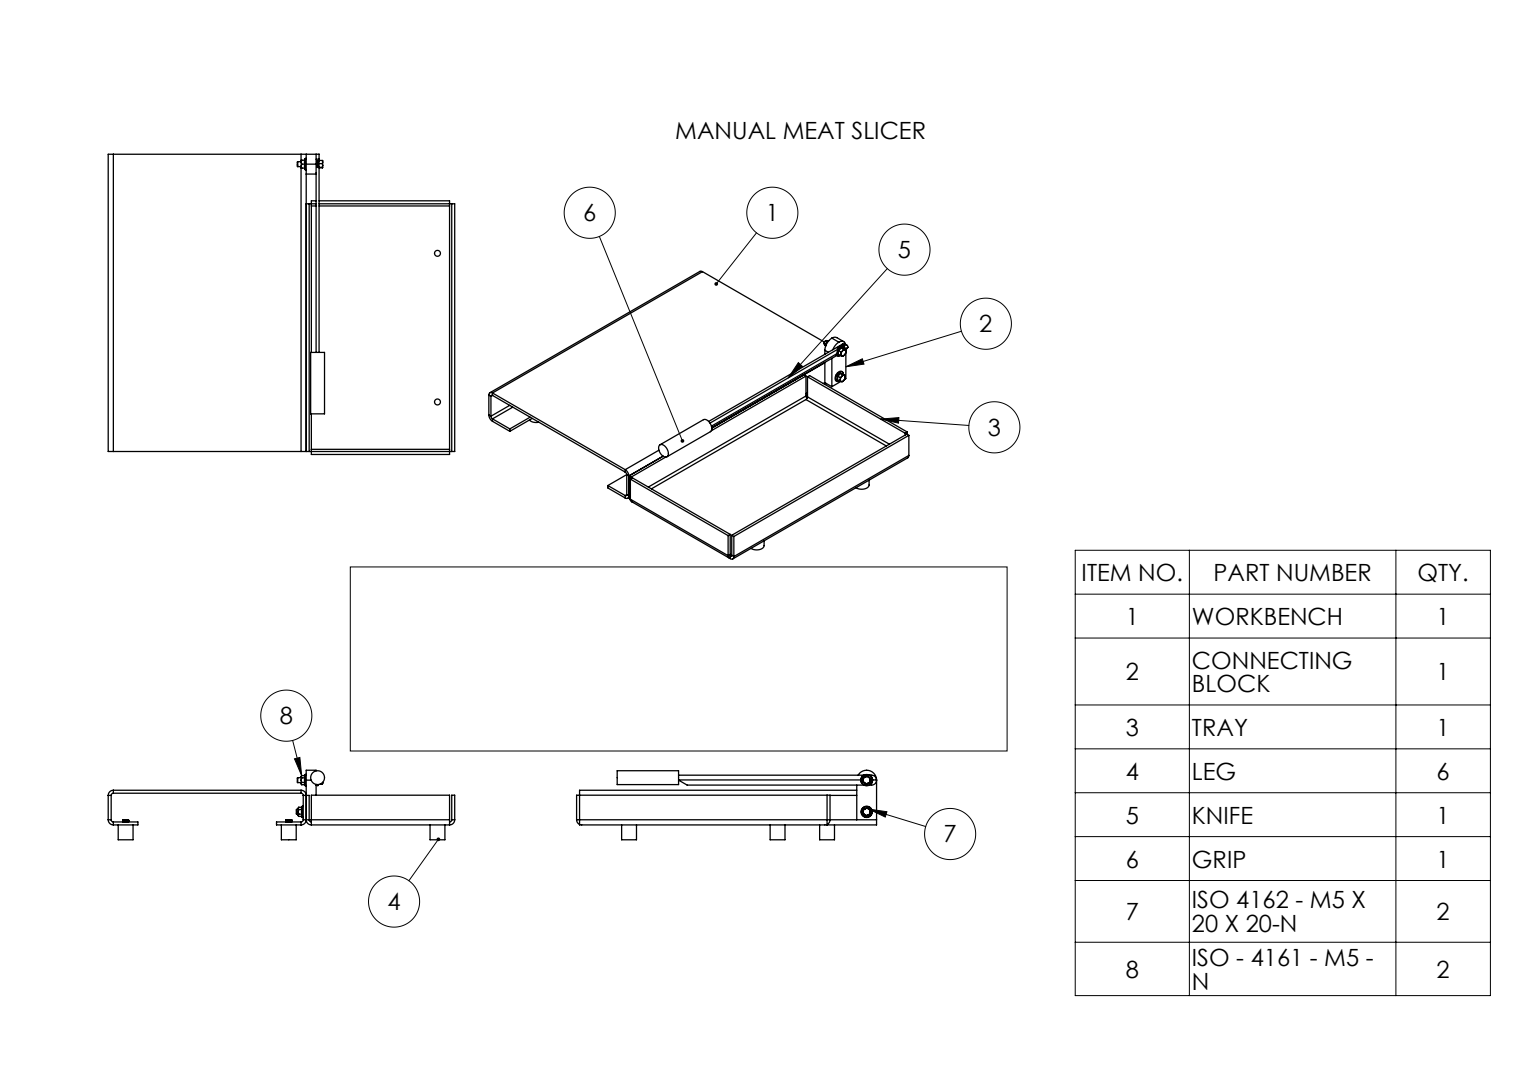
ISO-10303-21;
HEADER;
FILE_DESCRIPTION (('STEP AP214'),
    '1' );
FILE_NAME ('MAS-172',
    '2026-10-25T17:17:34',
    ( '' ),
    ( '' ),
    'SwSTEP 2.0',
    'SolidWorks 2026',
    '' );
FILE_SCHEMA (( 'AUTOMOTIVE_DESIGN' ));
ENDSEC;

DATA;
#1 = CARTESIAN_POINT ( 'NONE',  ( -79.64356964375001269, -33.59062499938548285, 98.40857419181659793 ) ) ;
#2 = CARTESIAN_POINT ( 'NONE',  ( 85.15643035625001289, -33.70312499938548711, 98.40857419181659793 ) ) ;
#3 = CARTESIAN_POINT ( 'NONE',  ( 82.39999999999999147, -32.36250000000000426, -96.99999999999997158 ) ) ;
#4 = DIRECTION ( 'NONE',  ( -0.000000000000000000, 0.8660254037844382635, 0.5000000000000006661 ) ) ;
#5 = CARTESIAN_POINT ( 'NONE',  ( 80.90000000000000568, -33.24374999877097281, -97.40192378864668399 ) ) ;
#6 = CARTESIAN_POINT ( 'NONE',  ( 231.0999999999999375, -32.62499999999999289, 102.5980762113533018 ) ) ;
#7 =( BOUNDED_SURFACE ( )  B_SPLINE_SURFACE ( 3, 2, ( 
 ( #3858, #16070, #12849 ),
 ( #17539, #18820, #1124 ),
 ( #12942, #8258, #11381 ),
 ( #11576, #9821, #15783 ),
 ( #19010, #5241, #9923 ),
 ( #17252, #845, #14308 ) ),
 .UNSPECIFIED., .F., .F., .F. ) 
 B_SPLINE_SURFACE_WITH_KNOTS ( ( 4, 2, 4 ),
 ( 3, 3 ),
 ( 0.02032853247518126918, 0.02278863295364821906, 0.02524873343211517240 ),
 ( 0.000000000000000000, 1.000000000000000000 ),
 .UNSPECIFIED. ) 
 GEOMETRIC_REPRESENTATION_ITEM ( )  RATIONAL_B_SPLINE_SURFACE ( (
 ( 1.000000000000000000, 0.8047781615896837382, 1.000000000000000000),
 ( 1.000000000000000000, 0.8123767586289252218, 1.000000000000000000),
 ( 1.000000000000000000, 0.8190662415564388121, 1.000000000000000000),
 ( 1.000000000000000000, 0.8192361015669026303, 1.000000000000000000),
 ( 1.000000000000000000, 0.8126135807103900266, 1.000000000000000000),
 ( 1.000000000000000000, 0.8047712338318593339, 1.000000000000000000) ) ) 
 REPRESENTATION_ITEM ( '' )  SURFACE ( )  );
#8 = ORIENTED_EDGE ( 'NONE', *, *, #12900, .F. ) ;
#9 = CARTESIAN_POINT ( 'NONE',  ( 4.175813232069147674, 2.061359961916367833, 3.570380186727398097 ) ) ;
#10 = CARTESIAN_POINT ( 'NONE',  ( 232.5999999999999375, -34.55624999877095860, 96.53589838486223584 ) ) ;
#11 = CARTESIAN_POINT ( 'NONE',  ( 234.0999999999999375, -32.34374999877096002, -52.59807621135342970 ) ) ;
#12 = CARTESIAN_POINT ( 'NONE',  ( -82.39999999999999147, -34.07812499938548711, 103.1828516163667899 ) ) ;
#13 = ORIENTED_EDGE ( 'NONE', *, *, #6864, .F. ) ;
#14 = VERTEX_POINT ( 'NONE', #6375 ) ;
#15 = CARTESIAN_POINT ( 'NONE',  ( -4.204015924366189871, 1.626724848190922446, -3.610627190413390419 ) ) ;
#16 = CARTESIAN_POINT ( 'NONE',  ( -85.39999999999999147, -34.97364041986484295, 98.90809577818235709 ) ) ;
#17 = CARTESIAN_POINT ( 'NONE',  ( -85.40000000000000568, -32.23124999877096997, 98.26794919243111792 ) ) ;
#18 = ORIENTED_EDGE ( 'NONE', *, *, #10099, .F. ) ;
#19 = CARTESIAN_POINT ( 'NONE',  ( -79.77811200999887831, -35.00000000000000000, 100.8506536761481414 ) ) ;
#20 = CARTESIAN_POINT ( 'NONE',  ( 82.40000000000000568, -30.00000000000000355, -103.0000000000000000 ) ) ;
#21 = CARTESIAN_POINT ( 'NONE',  ( -81.02178482187500208, -34.45312499938548711, 97.61286128772489690 ) ) ;
#22 = CARTESIAN_POINT ( 'NONE',  ( -79.39999999999999147, -33.41250000000000142, 101.7320508075688537 ) ) ;
#23 = CARTESIAN_POINT ( 'NONE',  ( -83.90000000000000568, -30.46874999877096712, 97.40192378864668399 ) ) ;
#24 = CARTESIAN_POINT ( 'NONE',  ( 231.7961524227065979, -33.50759618943233420, 103.0000000000000000 ) ) ;
#25 = CARTESIAN_POINT ( 'NONE',  ( 4.055492966679589806, 2.385006769472808319, 3.005124364834396822 ) ) ;
#26 = CARTESIAN_POINT ( 'NONE',  ( 0.000000000000000000, 0.000000000000000000, -0.2800830152838844622 ) ) ;
#27 = EDGE_CURVE ( 'NONE', #9630, #12897, #3914, .T. ) ;
#28 = CARTESIAN_POINT ( 'NONE',  ( 233.9782151781249411, -31.19062499938547717, 97.61286128772489690 ) ) ;
#29 = EDGE_LOOP ( 'NONE', ( #8971, #4412, #15076, #17801 ) ) ;
#30 = CARTESIAN_POINT ( 'NONE',  ( -85.15643035624999868, -34.22812499938547859, -101.5914258081833879 ) ) ;
#31 = CARTESIAN_POINT ( 'NONE',  ( 1.287237434362044075, 3.875615274277557809, -3.430618716626812059 ) ) ;
#32 = CARTESIAN_POINT ( 'NONE',  ( 233.4038475772933339, -34.57634618820330275, -53.00000000000011369 ) ) ;
#33 = CARTESIAN_POINT ( 'NONE',  ( 80.07894310789828296, -34.99999999999997868, -101.4973817956044400 ) ) ;
#34 = CARTESIAN_POINT ( 'NONE',  ( -85.15643035624999868, -31.00312499938548072, 101.5914258081833879 ) ) ;
#35 = CARTESIAN_POINT ( 'NONE',  ( 0.000000000000000000, 0.000000000000000000, -25.03750572909317285 ) ) ;
#36 = CARTESIAN_POINT ( 'NONE',  ( 233.9782151781249411, -32.54062499938547859, -52.38713871227520968 ) ) ;
#37 = ORIENTED_EDGE ( 'NONE', *, *, #1725, .T. ) ;
#38 = ORIENTED_EDGE ( 'NONE', *, *, #10348, .F. ) ;
#39 = CARTESIAN_POINT ( 'NONE',  ( -84.28136653320154892, -32.00000000000001421, 97.98546077809197641 ) ) ;
#40 = CARTESIAN_POINT ( 'NONE',  ( -85.40000000000000568, -31.38749999999999574, 98.26794919243111792 ) ) ;
#41 = CARTESIAN_POINT ( 'NONE',  ( -85.40000000000000568, -32.60624999877097707, 101.7320508075688679 ) ) ;
#42 = CARTESIAN_POINT ( 'NONE',  ( 82.39999999999999147, -32.36250000000000426, 103.4641016151377499 ) ) ;
#43 = CARTESIAN_POINT ( 'NONE',  ( -80.80636817121818183, -32.00000000000000000, -97.53037344451308854 ) ) ;
#44 = CARTESIAN_POINT ( 'NONE',  ( 235.3564303562499447, -33.92812499938548143, 98.40857419181659793 ) ) ;
#45 = CARTESIAN_POINT ( 'NONE',  ( 232.5999999999999943, -33.40312499938547575, -53.18285161636690361 ) ) ;
#46 = CARTESIAN_POINT ( 'NONE',  ( 82.39999999999999147, -33.62812499938549138, 96.81714838363319586 ) ) ;
#47 = EDGE_CURVE ( 'NONE', #12317, #11119, #12856, .T. ) ;
#48 = CARTESIAN_POINT ( 'NONE',  ( 85.15643035625001289, -30.59062499938548285, -99.99999999999998579 ) ) ;
#49 = ORIENTED_EDGE ( 'NONE', *, *, #18550, .F. ) ;
#50 =( BOUNDED_CURVE ( )  B_SPLINE_CURVE ( 2, ( #14072, #3327, #4905, #3619, #6463, #18477, #9481, #10851, #12417 ),
 .UNSPECIFIED., .F., .F. ) 
 B_SPLINE_CURVE_WITH_KNOTS ( ( 3, 2, 2, 2, 3 ),
 ( 0.6041666666666666297, 0.6111111111111111605, 0.6250000000000000000, 0.6388888888888888395, 0.6458333333333332593 ),
 .UNSPECIFIED. ) 
 CURVE ( )  GEOMETRIC_REPRESENTATION_ITEM ( )  RATIONAL_B_SPLINE_CURVE ( ( 0.9330127018922192983, 0.9330127018922187432, 1.000000000000000000, 0.8660254037844387076, 1.000000000000000000, 0.8660254037844387076, 1.000000000000000000, 0.9330127018922198534, 0.9330127018922192983 ) ) 
 REPRESENTATION_ITEM ( '' )  );
#51 = CARTESIAN_POINT ( 'NONE',  ( 235.3564303562499447, -34.41562499938547859, -50.00000000000011369 ) ) ;
#52 = CARTESIAN_POINT ( 'NONE',  ( 232.5999999999999375, -33.20624999877097139, 97.00000000000000000 ) ) ;
#53 = CARTESIAN_POINT ( 'NONE',  ( 83.77821517812500929, -34.26562499938548711, -97.61286128772489690 ) ) ;
#54 = EDGE_CURVE ( 'NONE', #12568, #18235, #14634, .T. ) ;
#55 = CYLINDRICAL_SURFACE ( 'NONE', #7872, 3.000000000000002665 ) ;
#56 = CARTESIAN_POINT ( 'NONE',  ( 233.9782151781249411, -31.90312499938548285, -47.61286128772501769 ) ) ;
#57 =( BOUNDED_CURVE ( )  B_SPLINE_CURVE ( 2, ( #14794, #2683, #1229, #10402, #2880, #14892, #1421, #4162, #17640 ),
 .UNSPECIFIED., .F., .F. ) 
 B_SPLINE_CURVE_WITH_KNOTS ( ( 3, 2, 2, 2, 3 ),
 ( 0.6458333333333333703, 0.6527777777777777901, 0.6666666666666666297, 0.6805555555555555802, 0.6875000000000000000 ),
 .UNSPECIFIED. ) 
 CURVE ( )  GEOMETRIC_REPRESENTATION_ITEM ( )  RATIONAL_B_SPLINE_CURVE ( ( 0.9330127018922192983, 0.9330127018922198534, 1.000000000000000000, 0.8660254037844387076, 1.000000000000000000, 0.8660254037844387076, 1.000000000000000000, 0.9330127018922194093, 0.9330127018922194093 ) ) 
 REPRESENTATION_ITEM ( '' )  );
#58 = CARTESIAN_POINT ( 'NONE',  ( -85.40000000000000568, -30.03750000000000497, 98.26794919243111792 ) ) ;
#59 = ORIENTED_EDGE ( 'NONE', *, *, #2774, .T. ) ;
#60 = CARTESIAN_POINT ( 'NONE',  ( -80.90000000000000568, -32.85000000000000142, 97.40192378864668399 ) ) ;
#61 = CARTESIAN_POINT ( 'NONE',  ( -79.39999999999999147, -31.03124999877097068, 98.26794919243110371 ) ) ;
#62 = DIRECTION ( 'NONE',  ( -0.000000000000000000, -0.000000000000000000, -1.000000000000000000 ) ) ;
#63 = CARTESIAN_POINT ( 'NONE',  ( -85.40000000000000568, -31.38356250001228531, 98.26794919243111792 ) ) ;
#64 = EDGE_CURVE ( 'NONE', #2579, #12229, #9687, .T. ) ;
#65 = LINE ( 'NONE', #3169, #11720 ) ;
#66 = PLANE ( 'NONE',  #10236 ) ;
#67 = CARTESIAN_POINT ( 'NONE',  ( -85.15643035624999868, -31.97812499938548925, 98.40857419181659793 ) ) ;
#68 = CARTESIAN_POINT ( 'NONE',  ( -79.39999999999999147, -32.47500000000000142, 99.99999999999998579 ) ) ;
#69 = CARTESIAN_POINT ( 'NONE',  ( 83.77821517812500929, -32.57812499938548711, 102.3871387122750889 ) ) ;
#70 = EDGE_CURVE ( 'NONE', #5083, #2374, #8515, .T. ) ;
#71 = B_SPLINE_CURVE_WITH_KNOTS ( 'NONE', 3,
 ( #6677, #3729, #9694, #17123, #815, #2842, #14458, #7240, #5600, #9889, #2460, #18880, #18782, #15852, #1291, #17315, #16038, #17507 ),
 .UNSPECIFIED., .F., .F.,
 ( 4, 2, 2, 2, 2, 2, 2, 2, 4 ),
 ( 0.000000000000000000, 0.0007106627595359568412, 0.001421325519071913682, 0.002131988278607870740, 0.002842651038143827365, 0.003553313797679783989, 0.004263976557215741481, 0.004974639316751698105, 0.005685302076287654729 ),
 .UNSPECIFIED. ) ;
#72 = CARTESIAN_POINT ( 'NONE',  ( 85.15643035625001289, -30.25312499938548783, -99.99999999999998579 ) ) ;
#73 = DIRECTION ( 'NONE',  ( -0.000000000000000000, -1.000000000000000000, -0.000000000000000000 ) ) ;
#74 = CARTESIAN_POINT ( 'NONE',  ( -83.77821517812500929, -32.87812499938548427, 102.3871387122750889 ) ) ;
#75 = CARTESIAN_POINT ( 'NONE',  ( -85.15643035624999868, -30.29062499938548925, -101.5914258081833879 ) ) ;
#76 = ORIENTED_EDGE ( 'NONE', *, *, #18961, .F. ) ;
#77 = CARTESIAN_POINT ( 'NONE',  ( 85.40000000000000568, -35.34374999877096712, 99.99999999999998579 ) ) ;
#78 = PLANE ( 'NONE',  #7094 ) ;
#79 = CARTESIAN_POINT ( 'NONE',  ( -82.40000000000000568, -30.00000000000000355, -96.99999999999998579 ) ) ;
#80 = VECTOR ( 'NONE', #9829, 1000.000000000000000 ) ;
#81 = CARTESIAN_POINT ( 'NONE',  ( -99.99999999999998579, -5.200000000000000178, 150.0000000000000000 ) ) ;
#82 = AXIS2_PLACEMENT_3D ( 'NONE', #16514, #3117, #16700 ) ;
#83 = CARTESIAN_POINT ( 'NONE',  ( -83.77821517812500929, -31.07812499938548711, 102.3871387122750889 ) ) ;
#84 =( BOUNDED_CURVE ( )  B_SPLINE_CURVE ( 2, ( #13183, #17688, #10354, #13091, #8980, #17790, #14840, #19061, #2929 ),
 .UNSPECIFIED., .F., .F. ) 
 B_SPLINE_CURVE_WITH_KNOTS ( ( 3, 2, 2, 2, 3 ),
 ( 0.7708333333333332593, 0.7777777777777777901, 0.7916666666666666297, 0.8055555555555555802, 0.8125000000000000000 ),
 .UNSPECIFIED. ) 
 CURVE ( )  GEOMETRIC_REPRESENTATION_ITEM ( )  RATIONAL_B_SPLINE_CURVE ( ( 0.9330127018922192983, 0.9330127018922187432, 1.000000000000000000, 0.8660254037844387076, 1.000000000000000000, 0.8660254037844387076, 1.000000000000000000, 0.9330127018922194093, 0.9330127018922194093 ) ) 
 REPRESENTATION_ITEM ( '' )  );
#85 = CARTESIAN_POINT ( 'NONE',  ( 82.61711639273572416, -31.99999999999999289, 102.8399189874672857 ) ) ;
#86 = ORIENTED_EDGE ( 'NONE', *, *, #4961, .F. ) ;
#87 = CARTESIAN_POINT ( 'NONE',  ( -83.90000000000000568, -30.82500000000000284, -97.40192378864668399 ) ) ;
#88 = CARTESIAN_POINT ( 'NONE',  ( 105.2000000000000455, -29.80000000000002203, 147.7999999999999829 ) ) ;
#89 = DIRECTION ( 'NONE',  ( 1.201851678989726239E-15, 0.8660254037844380415, -0.5000000000000009992 ) ) ;
#90 = CARTESIAN_POINT ( 'NONE',  ( -85.15643035625001289, -32.95312499938548711, -99.99999999999998579 ) ) ;
#91 = CARTESIAN_POINT ( 'NONE',  ( -82.14831453747900980, -32.00000000000000711, -102.8584433575392438 ) ) ;
#92 = CARTESIAN_POINT ( 'NONE',  ( 229.8435696437499303, -31.60312499938548214, 99.99999999999998579 ) ) ;
#93 = CARTESIAN_POINT ( 'NONE',  ( -79.39999999999999147, -32.91018749875867400, 101.7320508075688537 ) ) ;
#94 = APPLICATION_CONTEXT ( 'automotive_design' ) ;
#95 = CARTESIAN_POINT ( 'NONE',  ( -82.39999999999999147, -34.19062499938548427, 103.1828516163667899 ) ) ;
#96 = CARTESIAN_POINT ( 'NONE',  ( 233.4038475772933339, -33.67634618820329706, 96.99999999999998579 ) ) ;
#97 = CARTESIAN_POINT ( 'NONE',  ( 83.77821517812500929, -33.66562499938548569, 97.61286128772489690 ) ) ;
#98 = CARTESIAN_POINT ( 'NONE',  ( 80.90000000000000568, -32.40000000000000568, -97.40192378864668399 ) ) ;
#99 = AXIS2_PLACEMENT_3D ( 'NONE', #13083, #5582, #10259 ) ;
#100 = CARTESIAN_POINT ( 'NONE',  ( 232.5999999999999375, -33.43124999877096570, 102.9999999999999858 ) ) ;
#101 = EDGE_CURVE ( 'NONE', #1894, #1510, #1410, .T. ) ;
#102 = CARTESIAN_POINT ( 'NONE',  ( 83.90000000000000568, -35.26874999877097139, -102.5980762113533018 ) ) ;
#103 = CARTESIAN_POINT ( 'NONE',  ( 232.5999999999999375, -34.61249999999999716, 96.53589838486223584 ) ) ;
#104 = VERTEX_POINT ( 'NONE', #17014 ) ;
#105 = CARTESIAN_POINT ( 'NONE',  ( 231.2217848218749339, -34.22812499938548569, -47.61286128772501769 ) ) ;
#106 = DIRECTION ( 'NONE',  ( 0.000000000000000000, 0.000000000000000000, 1.000000000000000000 ) ) ;
#107 = CARTESIAN_POINT ( 'NONE',  ( 233.9782151781249411, -30.55312499938548143, 102.3871387122750889 ) ) ;
#108 = CARTESIAN_POINT ( 'NONE',  ( 229.5999999999999375, -33.99374999877096570, -50.00000000000011369 ) ) ;
#109 = CARTESIAN_POINT ( 'NONE',  ( -79.64356964374998427, -33.10312499938548569, 101.5914258081833879 ) ) ;
#110 = ORIENTED_EDGE ( 'NONE', *, *, #1169, .T. ) ;
#112 = ORIENTED_EDGE ( 'NONE', *, *, #10203, .F. ) ;
#111 = EDGE_CURVE ( 'NONE', #18607, #16633, #16646, .T. ) ;
#113 = CARTESIAN_POINT ( 'NONE',  ( -81.90908125319960220, -32.00000000000000711, 97.16185054498753004 ) ) ;
#114 = AXIS2_PLACEMENT_3D ( 'NONE', #4493, #4109, #5965 ) ;
#115 = CARTESIAN_POINT ( 'NONE',  ( -82.39999999999999147, -34.83749999999999858, 103.0000000000000000 ) ) ;
#116 = CARTESIAN_POINT ( 'NONE',  ( -79.39999999999999147, -34.76250000000000284, 101.7320508075688537 ) ) ;
#117 = ORIENTED_EDGE ( 'NONE', *, *, #1142, .T. ) ;
#118 = CARTESIAN_POINT ( 'NONE',  ( 69.99999999999998579, -31.99999999999998579, 150.0000000000000000 ) ) ;
#119 = CARTESIAN_POINT ( 'NONE',  ( 232.5999999999999375, -32.36249999999999716, 97.00000000000000000 ) ) ;
#120 = CARTESIAN_POINT ( 'NONE',  ( -85.15643035624999868, -33.44062499938548427, 98.40857419181659793 ) ) ;
#121 = CARTESIAN_POINT ( 'NONE',  ( -83.90000000000000568, -34.57500000000000284, 97.40192378864668399 ) ) ;
#122 = CARTESIAN_POINT ( 'NONE',  ( -79.39999999999999147, -31.93124999877096926, 98.26794919243110371 ) ) ;
#123 = FACE_OUTER_BOUND ( 'NONE', #5516, .T. ) ;
#124 =( BOUNDED_SURFACE ( )  B_SPLINE_SURFACE ( 1, 2, ( 
 ( #72, #18045, #10508, #17940, #4551, #3080, #4656, #1713, #12454, #13815, #2197, #651, #7770, #5135, #16858, #3463, #457, #16755, #7864, #15189, #8158, #2001, #1806, #6406, #9522, #9323, #14107, #17050, #9225, #11080, #551, #3563, #9626, #9421, #3371, #6508, #18420, #5041, #15389, #15287, #4754, #4848, #1902, #10982, #8060, #13913, #2100, #4947, #3269, #18518, #15588, #14015, #6599, #13723, #10793, #6699, #18329, #3661, #12361, #10890, #7958, #744, #364, #6313, #18135, #12266, #16951, #15487, #12547, #18231, #10698, #16664, #18617, #11277, #3951, #5339, #19004, #9815, #8536, #840, #5526, #6893, #1218, #6984, #14302, #2574, #12935, #5624, #16064, #14392, #1117, #18907, #15777, #18717, #3852, #17245, #2386, #12643, #12749, #8348, #11474, #4052, #15878, #938, #17441, #15685, #4148, #5235, #6803, #12843, #2482, #11183, #8440, #8253, #14486, #9719, #10011, #18812, #2669, #7077, #2289, #11570, #11375, #17341, #5436, #9916, #1031, #14203, #8629, #15969, #13033, #17533, #10108, #14587, #17147 ),
 ( #3754, #18022, #5908, #5808, #8918, #14880, #1509, #17822, #17733, #13124, #13221, #4340, #48, #16450, #2963, #10487, #13318, #11665, #7554, #4636, #3060, #9022, #16165, #19193, #15075, #7362, #148, #11759, #19295, #10301, #13511, #17628, #2776, #6099, #10201, #10391, #7459, #13419, #1318, #4243, #8729, #19094, #16260, #4433, #2870, #12047, #8827, #14981, #14683, #6000, #1409, #7174, #11950, #14784, #1605, #17920, #10586, #16551, #4529, #3150, #9113, #11854, #16352, #5715, #7266, #7751, #9602, #1786, #6293, #530, #12435, #4925, #16736, #15366, #4730, #12527, #7646, #15169, #15268, #10870, #13706, #6483, #3544, #1982, #15468, #346, #18116, #1883, #2078, #8035, #1694, #6581, #13601, #18403, #11059, #13992, #12244, #18211, #10964, #7940, #10772, #12341, #631, #3346, #5023, #4831, #18500, #9306, #10675, #440, #16841, #16644, #3447, #13891, #9500, #7842, #3640, #3246, #16934, #5119, #13797, #6385, #18305, #17030, #9402, #242, #6201, #12148, #9204, #17221, #8136, #18982, #17420, #4123, #2271 ) ),
 .UNSPECIFIED., .F., .F., .F. ) 
 B_SPLINE_SURFACE_WITH_KNOTS ( ( 2, 2 ),
 ( 3, 2, 2, 2, 2, 2, 2, 2, 2, 2, 2, 2, 2, 2, 2, 2, 2, 2, 2, 2, 2, 2, 2, 2, 2, 2, 2, 2, 2, 2, 2, 2, 2, 2, 2, 2, 2, 2, 2, 2, 2, 2, 2, 2, 2, 2, 2, 2, 2, 2, 2, 2, 2, 2, 2, 2, 2, 2, 2, 2, 2, 2, 2, 2, 2, 2, 2, 3 ),
 ( 0.000000000000000000, 1.000000000000000000 ),
 ( 0.000000000000000000, 0.01388888888888888812, 0.02777777777777777624, 0.04166666666666666435, 0.05555555555555555247, 0.06944444444444444753, 0.08333333333333332871, 0.09722222222222222376, 0.1111111111111111049, 0.1250000000000000000, 0.1388888888888888951, 0.1527777777777777901, 0.1666666666666666574, 0.1805555555555555525, 0.1944444444444444475, 0.2083333333333333426, 0.2222222222222222099, 0.2361111111111111049, 0.2500000000000000000, 0.2638888888888888951, 0.2777777777777777901, 0.2916666666666666852, 0.3055555555555555802, 0.3194444444444444198, 0.3333333333333333148, 0.3472222222222222099, 0.3611111111111111049, 0.3750000000000000000, 0.3888888888888888951, 0.4027777777777777901, 0.4166666666666666852, 0.4305555555555555802, 0.4444444444444444198, 0.4583333333333333148, 0.4722222222222222099, 0.4861111111111111049, 0.5000000000000000000, 0.5138888888888888395, 0.5277777777777777901, 0.5416666666666666297, 0.5555555555555555802, 0.5694444444444444198, 0.5833333333333333703, 0.5972222222222222099, 0.6111111111111111605, 0.6250000000000000000, 0.6388888888888888395, 0.6527777777777777901, 0.6666666666666666297, 0.6805555555555555802, 0.6944444444444444198, 0.7083333333333333703, 0.7222222222222222099, 0.7361111111111111605, 0.7500000000000000000, 0.7638888888888888395, 0.7777777777777777901, 0.7916666666666666297, 0.8055555555555555802, 0.8194444444444444198, 0.8333333333333333703, 0.8472222222222222099, 0.8611111111111111605, 0.8750000000000000000, 0.8888888888888888395, 0.9027777777777777901, 0.9166666666666666297, 0.9258785565094813652 ),
 .UNSPECIFIED. ) 
 GEOMETRIC_REPRESENTATION_ITEM ( )  RATIONAL_B_SPLINE_SURFACE ( (
 ( 1.000000000000000000, 0.8660254037844387076, 1.000000000000000000, 0.8660254037844387076, 1.000000000000000000, 0.8660254037844387076, 1.000000000000000000, 0.8660254037844387076, 1.000000000000000000, 0.8660254037844387076, 1.000000000000000000, 0.8660254037844387076, 1.000000000000000000, 0.8660254037844387076, 1.000000000000000000, 0.8660254037844387076, 1.000000000000000000, 0.8660254037844387076, 1.000000000000000000, 0.8660254037844387076, 1.000000000000000000, 0.8660254037844387076, 1.000000000000000000, 0.8660254037844387076, 1.000000000000000000, 0.8660254037844387076, 1.000000000000000000, 0.8660254037844387076, 1.000000000000000000, 0.8660254037844387076, 1.000000000000000000, 0.8660254037844387076, 1.000000000000000000, 0.8660254037844387076, 1.000000000000000000, 0.8660254037844387076, 1.000000000000000000, 0.8660254037844387076, 1.000000000000000000, 0.8660254037844387076, 1.000000000000000000, 0.8660254037844387076, 1.000000000000000000, 0.8660254037844387076, 1.000000000000000000, 0.8660254037844387076, 1.000000000000000000, 0.8660254037844387076, 1.000000000000000000, 0.8660254037844387076, 1.000000000000000000, 0.8660254037844387076, 1.000000000000000000, 0.8660254037844387076, 1.000000000000000000, 0.8660254037844387076, 1.000000000000000000, 0.8660254037844387076, 1.000000000000000000, 0.8660254037844387076, 1.000000000000000000, 0.8660254037844387076, 1.000000000000000000, 0.8660254037844387076, 1.000000000000000000, 0.8660254037844387076, 1.000000000000000000, 0.8660254037844387076, 1.000000000000000000, 0.8660254037844387076, 1.000000000000000000, 0.8660254037844387076, 1.000000000000000000, 0.8660254037844387076, 1.000000000000000000, 0.8660254037844387076, 1.000000000000000000, 0.8660254037844387076, 1.000000000000000000, 0.8660254037844387076, 1.000000000000000000, 0.8660254037844387076, 1.000000000000000000, 0.8660254037844387076, 1.000000000000000000, 0.8660254037844387076, 1.000000000000000000, 0.8660254037844387076, 1.000000000000000000, 0.8660254037844387076, 1.000000000000000000, 0.8660254037844387076, 1.000000000000000000, 0.8660254037844387076, 1.000000000000000000, 0.8660254037844387076, 1.000000000000000000, 0.8660254037844387076, 1.000000000000000000, 0.8660254037844387076, 1.000000000000000000, 0.8660254037844387076, 1.000000000000000000, 0.8660254037844387076, 1.000000000000000000, 0.8660254037844387076, 1.000000000000000000, 0.8660254037844387076, 1.000000000000000000, 0.8660254037844387076, 1.000000000000000000, 0.8660254037844387076, 1.000000000000000000, 0.8660254037844387076, 1.000000000000000000, 0.8660254037844387076, 1.000000000000000000, 0.8660254037844387076, 1.000000000000000000, 0.8660254037844387076, 1.000000000000000000, 0.8660254037844387076, 1.000000000000000000, 0.8660254037844387076, 1.000000000000000000, 0.8660254037844387076, 1.000000000000000000, 0.8660254037844387076, 1.000000000000000000, 0.8660254037844387076, 1.000000000000000000, 0.8660254037844387076, 1.000000000000000000, 0.9111405360107203144, 0.9401542295229963209),
 ( 1.000000000000000000, 0.8660254037844387076, 1.000000000000000000, 0.8660254037844387076, 1.000000000000000000, 0.8660254037844387076, 1.000000000000000000, 0.8660254037844387076, 1.000000000000000000, 0.8660254037844387076, 1.000000000000000000, 0.8660254037844387076, 1.000000000000000000, 0.8660254037844387076, 1.000000000000000000, 0.8660254037844387076, 1.000000000000000000, 0.8660254037844387076, 1.000000000000000000, 0.8660254037844387076, 1.000000000000000000, 0.8660254037844387076, 1.000000000000000000, 0.8660254037844387076, 1.000000000000000000, 0.8660254037844387076, 1.000000000000000000, 0.8660254037844387076, 1.000000000000000000, 0.8660254037844387076, 1.000000000000000000, 0.8660254037844387076, 1.000000000000000000, 0.8660254037844387076, 1.000000000000000000, 0.8660254037844387076, 1.000000000000000000, 0.8660254037844387076, 1.000000000000000000, 0.8660254037844387076, 1.000000000000000000, 0.8660254037844387076, 1.000000000000000000, 0.8660254037844387076, 1.000000000000000000, 0.8660254037844387076, 1.000000000000000000, 0.8660254037844387076, 1.000000000000000000, 0.8660254037844387076, 1.000000000000000000, 0.8660254037844387076, 1.000000000000000000, 0.8660254037844387076, 1.000000000000000000, 0.8660254037844387076, 1.000000000000000000, 0.8660254037844387076, 1.000000000000000000, 0.8660254037844387076, 1.000000000000000000, 0.8660254037844387076, 1.000000000000000000, 0.8660254037844387076, 1.000000000000000000, 0.8660254037844387076, 1.000000000000000000, 0.8660254037844387076, 1.000000000000000000, 0.8660254037844387076, 1.000000000000000000, 0.8660254037844387076, 1.000000000000000000, 0.8660254037844387076, 1.000000000000000000, 0.8660254037844387076, 1.000000000000000000, 0.8660254037844387076, 1.000000000000000000, 0.8660254037844387076, 1.000000000000000000, 0.8660254037844387076, 1.000000000000000000, 0.8660254037844387076, 1.000000000000000000, 0.8660254037844387076, 1.000000000000000000, 0.8660254037844387076, 1.000000000000000000, 0.8660254037844387076, 1.000000000000000000, 0.8660254037844387076, 1.000000000000000000, 0.8660254037844387076, 1.000000000000000000, 0.8660254037844387076, 1.000000000000000000, 0.8660254037844387076, 1.000000000000000000, 0.8660254037844387076, 1.000000000000000000, 0.8660254037844387076, 1.000000000000000000, 0.8660254037844387076, 1.000000000000000000, 0.8660254037844387076, 1.000000000000000000, 0.8660254037844387076, 1.000000000000000000, 0.8660254037844387076, 1.000000000000000000, 0.8660254037844387076, 1.000000000000000000, 0.8660254037844387076, 1.000000000000000000, 0.8660254037844387076, 1.000000000000000000, 0.8660254037844387076, 1.000000000000000000, 0.8660254037844387076, 1.000000000000000000, 0.8660254037844387076, 1.000000000000000000, 0.8660254037844387076, 1.000000000000000000, 0.8660254037844387076, 1.000000000000000000, 0.8660254037844387076, 1.000000000000000000, 0.8660254037844387076, 1.000000000000000000, 0.8660254037844387076, 1.000000000000000000, 0.9111405360107203144, 0.9401542295229963209) ) ) 
 REPRESENTATION_ITEM ( '' )  SURFACE ( )  );
#125 = CARTESIAN_POINT ( 'NONE',  ( 234.0999999999999375, -33.29999999999999716, 97.40192378864668399 ) ) ;
#126 = CARTESIAN_POINT ( 'NONE',  ( -80.90000000000000568, -33.45000000000000284, 102.5980762113533018 ) ) ;
#127 = CARTESIAN_POINT ( 'NONE',  ( -79.39999999999999147, -34.70624999877097139, -98.26794919243113213 ) ) ;
#128 = CARTESIAN_POINT ( 'NONE',  ( 229.8435696437499303, -31.04062499938547859, 99.99999999999998579 ) ) ;
#129 = ORIENTED_EDGE ( 'NONE', *, *, #8766, .F. ) ;
#130 = SHAPE_REPRESENTATION_RELATIONSHIP ( 'NONE' , 'NONE' ,  #4499, #5537 ) ;
#131 = CARTESIAN_POINT ( 'NONE',  ( -79.64356964374999848, -33.51562499938548711, -99.99999999999998579 ) ) ;
#132 = CARTESIAN_POINT ( 'NONE',  ( -82.65380294351676582, -34.99990492518305274, 97.01075526832239859 ) ) ;
#133 = CARTESIAN_POINT ( 'NONE',  ( 233.4038475772933054, -34.76115380933863008, -47.00000000000011369 ) ) ;
#134 = CARTESIAN_POINT ( 'NONE',  ( 81.96801452314025482, -35.00000000000000000, -102.7281823352556671 ) ) ;
#135 = CARTESIAN_POINT ( 'NONE',  ( -81.02178482187500208, -31.19062499938548427, 97.61286128772489690 ) ) ;
#136 = FACE_OUTER_BOUND ( 'NONE', #875, .T. ) ;
#137 = CARTESIAN_POINT ( 'NONE',  ( 233.9782151781249411, -32.24062499938548143, -47.61286128772501769 ) ) ;
#138 = VERTEX_POINT ( 'NONE', #3624 ) ;
#139 = EDGE_LOOP ( 'NONE', ( #12823, #17187, #7892, #9526 ) ) ;
#140 = CARTESIAN_POINT ( 'NONE',  ( -5.488773498207864225E-16, -2.859595677584339413, 2.047034997319579386 ) ) ;
#141 = CARTESIAN_POINT ( 'NONE',  ( -79.39999999999999147, -30.26249999999999929, 101.7320508075688537 ) ) ;
#142 = CARTESIAN_POINT ( 'NONE',  ( -79.39999999999999147, -32.90624999877096712, 101.7320508075688537 ) ) ;
#143 = CARTESIAN_POINT ( 'NONE',  ( 80.90000000000000568, -31.50000000000000000, 102.5980762113533018 ) ) ;
#144 = CARTESIAN_POINT ( 'NONE',  ( 244.7999999999999545, -32.00000000000000000, -100.0000000000000000 ) ) ;
#145 = CARTESIAN_POINT ( 'NONE',  ( 231.2217848218749339, -34.71562499938547575, 97.61286128772489690 ) ) ;
#146 = CARTESIAN_POINT ( 'NONE',  ( 83.90000000000000568, -32.11874999877097281, 97.40192378864668399 ) ) ;
#147 = CARTESIAN_POINT ( 'NONE',  ( 79.39999999999999147, -33.33749999999999858, -98.26794919243110371 ) ) ;
#148 = CARTESIAN_POINT ( 'NONE',  ( 83.77821517812500929, -31.11562499938548498, -97.61286128772489690 ) ) ;
#149 = ORIENTED_EDGE ( 'NONE', *, *, #9637, .F. ) ;
#150 = CARTESIAN_POINT ( 'NONE',  ( 235.5999999999999375, -32.47499999999999432, -50.00000000000011369 ) ) ;
#151 = CARTESIAN_POINT ( 'NONE',  ( 82.40000000000000568, -34.10624999877096997, 102.9999999999999858 ) ) ;
#152 = CARTESIAN_POINT ( 'NONE',  ( 79.64356964375001269, -34.37812499938548427, -98.40857419181659793 ) ) ;
#153 = CARTESIAN_POINT ( 'NONE',  ( -1.935715396507168721E-15, 2.686816014504566752, 2.346298152288372130 ) ) ;
#154 = CARTESIAN_POINT ( 'NONE',  ( -81.59615242270662350, -34.76115380933863719, 103.0000000000000000 ) ) ;
#155 = CARTESIAN_POINT ( 'NONE',  ( 229.8435696437499871, -31.11562499938547788, -48.40857419181671162 ) ) ;
#156 = CARTESIAN_POINT ( 'NONE',  ( -79.39999999999999147, -31.08750000000000213, 98.26794919243110371 ) ) ;
#157 = ORIENTED_EDGE ( 'NONE', *, *, #9586, .F. ) ;
#158 = DIRECTION ( 'NONE',  ( 0.000000000000000000, 1.000000000000000000, 0.000000000000000000 ) ) ;
#159 = CARTESIAN_POINT ( 'NONE',  ( 233.9782151781249411, -34.94062499938547717, 102.3871387122750889 ) ) ;
#160 = CARTESIAN_POINT ( 'NONE',  ( -79.39999999999999147, -32.43356250001229313, 98.26794919243110371 ) ) ;
#161 = EDGE_CURVE ( 'NONE', #11737, #9031, #8962, .T. ) ;
#162 = EDGE_CURVE ( 'NONE', #9344, #9023, #15270, .T. ) ;
#163 = DIRECTION ( 'NONE',  ( 1.000000000000000000, 0.000000000000000000, 0.000000000000000000 ) ) ;
#164 = CARTESIAN_POINT ( 'NONE',  ( -82.40000000000000568, -32.30624999877097281, 97.00000000000000000 ) ) ;
#165 = CARTESIAN_POINT ( 'NONE',  ( 230.0248882325332147, -35.00000000000000711, 98.48300226792288470 ) ) ;
#166 = CARTESIAN_POINT ( 'NONE',  ( 81.02178482187500208, -34.90312499938548285, 102.3871387122750889 ) ) ;
#167 = DIRECTION ( 'NONE',  ( 0.000000000000000000, 0.000000000000000000, 1.000000000000000000 ) ) ;
#168 = CARTESIAN_POINT ( 'NONE',  ( 0.000000000000000000, 0.000000000000000000, 0.000000000000000000 ) ) ;
#169 = CARTESIAN_POINT ( 'NONE',  ( -83.77821517812500929, -32.42812499938548854, 102.3871387122750889 ) ) ;
#170 = CARTESIAN_POINT ( 'NONE',  ( -81.02178482187500208, -30.55312499938548854, -97.61286128772489690 ) ) ;
#171 =( BOUNDED_CURVE ( )  B_SPLINE_CURVE ( 2, ( #17183, #11218, #2322, #15621, #3787, #16002, #5563, #9753, #17473 ),
 .UNSPECIFIED., .F., .F. ) 
 B_SPLINE_CURVE_WITH_KNOTS ( ( 3, 2, 2, 2, 3 ),
 ( 0.7291666666666668517, 0.7361111111111111605, 0.7500000000000000000, 0.7638888888888888395, 0.7708333333333332593 ),
 .UNSPECIFIED. ) 
 CURVE ( )  GEOMETRIC_REPRESENTATION_ITEM ( )  RATIONAL_B_SPLINE_CURVE ( ( 0.9330127018922194093, 0.9330127018922209636, 1.000000000000000000, 0.8660254037844387076, 1.000000000000000000, 0.8660254037844387076, 1.000000000000000000, 0.9330127018922198534, 0.9330127018922192983 ) ) 
 REPRESENTATION_ITEM ( '' )  );
#172 = ORIENTED_EDGE ( 'NONE', *, *, #15080, .F. ) ;
#173 = CARTESIAN_POINT ( 'NONE',  ( 83.77821517812500929, -31.07812499938548711, 97.61286128772489690 ) ) ;
#174 = CARTESIAN_POINT ( 'NONE',  ( -94.79999999999999716, -35.00000000000000000, 150.0000000000000000 ) ) ;
#175 = EDGE_CURVE ( 'NONE', #12231, #5767, #14452, .T. ) ;
#176 = VECTOR ( 'NONE', #9077, 1000.000000000000000 ) ;
#177 = SURFACE_SIDE_STYLE ('',( #16764 ) ) ;
#178 = EDGE_CURVE ( 'NONE', #2762, #9031, #12708, .T. ) ;
#179 = CARTESIAN_POINT ( 'NONE',  ( -81.02178482187500208, -31.30312499938548498, 97.61286128772489690 ) ) ;
#180 = CARTESIAN_POINT ( 'NONE',  ( 109.9999999999999432, -29.80000000000002558, -150.0000000000000000 ) ) ;
#181 = ORIENTED_EDGE ( 'NONE', *, *, #9607, .T. ) ;
#182 = CARTESIAN_POINT ( 'NONE',  ( -79.39999999999999147, -32.06250000000000000, -98.26794919243113213 ) ) ;
#183 = CARTESIAN_POINT ( 'NONE',  ( 4.000000000000000000, 2.512223110932545023, -3.469391141908803711 ) ) ;
#184 = DIRECTION ( 'NONE',  ( 1.000000000000000000, -2.001604010742470847E-15, 0.000000000000000000 ) ) ;
#185 = CARTESIAN_POINT ( 'NONE',  ( -81.02178482187500208, -32.35312499938548569, -97.61286128772489690 ) ) ;
#186 = CARTESIAN_POINT ( 'NONE',  ( 232.5999999999999375, -34.61249999999999716, -53.00000000000011369 ) ) ;
#187 = EDGE_CURVE ( 'NONE', #10576, #17634, #10361, .T. ) ;
#188 = CARTESIAN_POINT ( 'NONE',  ( 233.9782151781249411, -32.35312499938547859, 102.3871387122750889 ) ) ;
#189 = CARTESIAN_POINT ( 'NONE',  ( -80.90000000000000568, -32.49768749875867968, 102.5980762113533018 ) ) ;
#190 = CARTESIAN_POINT ( 'NONE',  ( -83.77821517812500929, -33.02812499938548285, 97.61286128772489690 ) ) ;
#191 = CARTESIAN_POINT ( 'NONE',  ( -85.15643035625001289, -34.60312499938548569, -98.40857419181659793 ) ) ;
#192 = CARTESIAN_POINT ( 'NONE',  ( 85.15643035625001289, -34.22812499938548569, 101.5914258081833879 ) ) ;
#193 = CARTESIAN_POINT ( 'NONE',  ( -5.384454397937118664, 6.702023979852544604E-16, -5.000000000000000000 ) ) ;
#194 = CIRCLE ( 'NONE', #8915, 2.199999999999993516 ) ;
#195 = DIRECTION ( 'NONE',  ( 1.000000000000000000, 0.000000000000000000, -0.000000000000000000 ) ) ;
#196 = CARTESIAN_POINT ( 'NONE',  ( 82.39999999999999147, -33.43124999877097281, -103.4641016151377499 ) ) ;
#197 = CARTESIAN_POINT ( 'NONE',  ( 235.5999999999999943, -34.76249999999999574, 101.7320508075688537 ) ) ;
#198 = VERTEX_POINT ( 'NONE', #5871 ) ;
#199 = CARTESIAN_POINT ( 'NONE',  ( 231.2217848218749339, -34.37812499938547717, -52.38713871227520968 ) ) ;
#200 = CARTESIAN_POINT ( 'NONE',  ( 116.6000000000000085, 10.19999999999994600, -140.0000000000000000 ) ) ;
#201 = CARTESIAN_POINT ( 'NONE',  ( 229.8435696437499871, -30.66562499938547859, 101.5914258081833879 ) ) ;
#202 = CARTESIAN_POINT ( 'NONE',  ( 229.5999999999999375, -33.95624999877095718, -48.26794919243123161 ) ) ;
#203 = CARTESIAN_POINT ( 'NONE',  ( -83.77821517812500929, -33.36562499938548854, 97.61286128772489690 ) ) ;
#204 = EDGE_LOOP ( 'NONE', ( #12601, #4330, #15037, #10087 ) ) ;
#205 = ORIENTED_EDGE ( 'NONE', *, *, #14467, .T. ) ;
#206 = CARTESIAN_POINT ( 'NONE',  ( 4.071447262713887127, 2.020725942163686728, -3.499999999999999556 ) ) ;
#207 = CARTESIAN_POINT ( 'NONE',  ( 105.1999999999999886, -29.80000000000002203, -100.0000000000000142 ) ) ;
#208 = ORIENTED_EDGE ( 'NONE', *, *, #11264, .T. ) ;
#209 = FACE_OUTER_BOUND ( 'NONE', #12612, .T. ) ;
#210 = CARTESIAN_POINT ( 'NONE',  ( 99.99999999999994316, -29.80000000000000782, -150.0000000000000000 ) ) ;
#211 = CARTESIAN_POINT ( 'NONE',  ( -85.15643035625001289, -33.40312499938548285, 99.99999999999998579 ) ) ;
#212 = CARTESIAN_POINT ( 'NONE',  ( -85.40000000000000568, -30.35045094645306563, 101.9998975609119469 ) ) ;
#213 = CARTESIAN_POINT ( 'NONE',  ( -82.39999999999999147, -30.73124999877096641, 103.4641016151377499 ) ) ;
#214 = CARTESIAN_POINT ( 'NONE',  ( 229.5999999999999375, -33.60000000000000142, 99.99999999999998579 ) ) ;
#215 = AXIS2_PLACEMENT_3D ( 'NONE', #7607, #13659, #15226 ) ;
#216 = CARTESIAN_POINT ( 'NONE',  ( -82.39999999999999147, -35.09062499938548285, 103.1828516163667899 ) ) ;
#217 = EDGE_CURVE ( 'NONE', #4443, #15882, #16415, .T. ) ;
#218 = CARTESIAN_POINT ( 'NONE',  ( 82.39999999999999147, -34.83749999999999858, -103.0000000000000000 ) ) ;
#219 = CARTESIAN_POINT ( 'NONE',  ( 3.948103430090399879, 3.379418997638482747, 1.146674596026232784 ) ) ;
#220 = CARTESIAN_POINT ( 'NONE',  ( -82.40000000000000568, -30.00000000000000355, -103.0000000000000000 ) ) ;
#221 = CARTESIAN_POINT ( 'NONE',  ( 235.3564303562499447, -32.16562499938547859, 99.99999999999998579 ) ) ;
#222 = ORIENTED_EDGE ( 'NONE', *, *, #5417, .T. ) ;
#223 = SHAPE_REPRESENTATION_RELATIONSHIP ( 'NONE' , 'NONE' ,  #14995, #14131 ) ;
#224 = CARTESIAN_POINT ( 'NONE',  ( -85.15643035625001289, -33.29062499938547859, -99.99999999999998579 ) ) ;
#225 = CARTESIAN_POINT ( 'NONE',  ( 3.453038570460273071, 2.625189405340834448, -3.535263753543585352 ) ) ;
#226 = CARTESIAN_POINT ( 'NONE',  ( 235.5999999999999375, -33.82499999999999574, 99.99999999999998579 ) ) ;
#227 = LINE ( 'NONE', #4417, #3668 ) ;
#228 = CARTESIAN_POINT ( 'NONE',  ( 230.7429016803109221, -35.00000000000000711, -47.88253972981398476 ) ) ;
#229 = LINE ( 'NONE', #334, #1662 ) ;
#230 = ORIENTED_EDGE ( 'NONE', *, *, #9491, .F. ) ;
#231 = ORIENTED_EDGE ( 'NONE', *, *, #3636, .T. ) ;
#232 = CARTESIAN_POINT ( 'NONE',  ( -83.74167325096719594, -31.99999999999997868, 102.4658751321106962 ) ) ;
#233 = CARTESIAN_POINT ( 'NONE',  ( -83.90000000000000568, -30.07499999999999929, 97.40192378864668399 ) ) ;
#234 = AXIS2_PLACEMENT_3D ( 'NONE', #19240, #195, #10724 ) ;
#235 = CARTESIAN_POINT ( 'NONE',  ( -83.90000000000000568, -30.91874999877096997, 97.40192378864668399 ) ) ;
#236 = CARTESIAN_POINT ( 'NONE',  ( 82.39999999999999147, -32.58750000000000568, 96.53589838486223584 ) ) ;
#237 = CARTESIAN_POINT ( 'NONE',  ( -80.42036527867321638, -32.00000000000000000, -97.80162405160960759 ) ) ;
#238 = CARTESIAN_POINT ( 'NONE',  ( 229.8435696437499303, -33.29062499938547148, 99.99999999999998579 ) ) ;
#239 = CARTESIAN_POINT ( 'NONE',  ( 231.7960411235079050, -35.00000000000002132, -47.36341917746382535 ) ) ;
#240 = VECTOR ( 'NONE', #19274, 1000.000000000000000 ) ;
#241 = CARTESIAN_POINT ( 'NONE',  ( 81.59615242270662350, -33.46740381056766722, -102.9999999999999716 ) ) ;
#242 = CARTESIAN_POINT ( 'NONE',  ( 79.64356964375001269, -34.82812499938548711, -98.40857419181659793 ) ) ;
#243 = ORIENTED_EDGE ( 'NONE', *, *, #11982, .F. ) ;
#244 = CARTESIAN_POINT ( 'NONE',  ( 229.5999999999999375, -32.21249999999999858, -48.26794919243123161 ) ) ;
#245 = CARTESIAN_POINT ( 'NONE',  ( -80.90000000000000568, -31.59374999877097423, 102.5980762113533018 ) ) ;
#246 = CARTESIAN_POINT ( 'NONE',  ( 85.15643035624999868, -33.77812499938548285, -98.40857419181659793 ) ) ;
#247 = VECTOR ( 'NONE', #7483, 1000.000000000000000 ) ;
#248 = STYLED_ITEM ( 'NONE', ( #13866 ), #18578 ) ;
#249 = CARTESIAN_POINT ( 'NONE',  ( 94.79999999999995453, -29.80000000000000071, 150.0000000000000000 ) ) ;
#250 = CARTESIAN_POINT ( 'NONE',  ( -83.77821517812500929, -31.52812499938548996, 102.3871387122750889 ) ) ;
#251 = CARTESIAN_POINT ( 'NONE',  ( 233.9782151781249411, -33.70312499938548001, -47.61286128772501769 ) ) ;
#252 = CARTESIAN_POINT ( 'NONE',  ( -80.90000000000000568, -30.75000000000000355, 102.5980762113533018 ) ) ;
#253 = ORIENTED_EDGE ( 'NONE', *, *, #17135, .F. ) ;
#254 = CARTESIAN_POINT ( 'NONE',  ( -82.31848699153323423, -34.99951142137499716, 103.0191144166183221 ) ) ;
#255 = ADVANCED_FACE ( 'NONE', ( #14648 ), #17592, .T. ) ;
#256 = AXIS2_PLACEMENT_3D ( 'NONE', #7391, #10235, #1349 ) ;
#257 = DIRECTION ( 'NONE',  ( 0.000000000000000000, 0.000000000000000000, -1.000000000000000000 ) ) ;
#258 = CARTESIAN_POINT ( 'NONE',  ( 79.64356964375001269, -30.85312499938548569, 98.40857419181659793 ) ) ;
#259 = CARTESIAN_POINT ( 'NONE',  ( -85.40000000000000568, -34.96970290221972277, 98.90809659374338025 ) ) ;
#260 = CIRCLE ( 'NONE', #11165, 5.000000000000000000 ) ;
#261 = CARTESIAN_POINT ( 'NONE',  ( -1.999999999999999556, 3.464101615137754830, -3.142992957459232795 ) ) ;
#262 = CARTESIAN_POINT ( 'NONE',  ( -79.64356964374998427, -30.51562499938548711, 101.5914258081833879 ) ) ;
#263 = CARTESIAN_POINT ( 'NONE',  ( 85.12124608221321864, -31.99999999999999289, 100.4735569575797030 ) ) ;
#264 = CARTESIAN_POINT ( 'NONE',  ( 83.77821517812500929, -33.92812499938548854, 102.3871387122750889 ) ) ;
#265 = CARTESIAN_POINT ( 'NONE',  ( -2.100000000000000089, 2.571758278209441957E-16, -5.000000000000000000 ) ) ;
#266 = AXIS2_PLACEMENT_3D ( 'NONE', #8263, #12758, #18727 ) ;
#267 = CARTESIAN_POINT ( 'NONE',  ( 235.5999999999999943, -32.96249999999999858, -48.26794919243124582 ) ) ;
#268 = CARTESIAN_POINT ( 'NONE',  ( -84.74067385206558356, -32.00000000000000000, -101.4666071953143529 ) ) ;
#269 = CARTESIAN_POINT ( 'NONE',  ( -79.64356964374999848, -34.52812499938548285, -99.99999999999998579 ) ) ;
#270 = PRODUCT_DEFINITION_CONTEXT ( 'detailed design', #8572, 'design' ) ;
#271 = ORIENTED_EDGE ( 'NONE', *, *, #3421, .F. ) ;
#272 = CARTESIAN_POINT ( 'NONE',  ( 79.64356964375001269, -31.41562499938548569, 98.40857419181659793 ) ) ;
#273 = CARTESIAN_POINT ( 'NONE',  ( 96.99999999999998579, 4.758098676964956264E-15, -150.0000000000000000 ) ) ;
#274 = AXIS2_PLACEMENT_3D ( 'NONE', #18067, #19141, #10151 ) ;
#275 = CARTESIAN_POINT ( 'NONE',  ( 4.114405500665261783, -2.025575754679711959, -3.508400121684924322 ) ) ;
#276 = VECTOR ( 'NONE', #14347, 1000.000000000000000 ) ;
#277 = CARTESIAN_POINT ( 'NONE',  ( -82.39999999999999147, -31.49062499938548854, 103.1828516163667899 ) ) ;
#278 = DIRECTION ( 'NONE',  ( 0.000000000000000000, -1.000000000000000000, 0.000000000000000000 ) ) ;
#279 = ORIENTED_EDGE ( 'NONE', *, *, #11777, .T. ) ;
#280 = CARTESIAN_POINT ( 'NONE',  ( -85.40000000000000568, -30.86250000000000071, -98.26794919243111792 ) ) ;
#281 = CARTESIAN_POINT ( 'NONE',  ( 85.40000000000000568, -34.46249999999999858, -101.7320508075688679 ) ) ;
#282 = DIRECTION ( 'NONE',  ( -1.000000000000000000, 0.000000000000000000, 0.000000000000000000 ) ) ;
#283 = CARTESIAN_POINT ( 'NONE',  ( -85.15643035624999868, -33.81562499938549138, -98.40857419181659793 ) ) ;
#284 = CARTESIAN_POINT ( 'NONE',  ( -0.5449313310646672903, -4.304185902836978883, -3.316620875263469159 ) ) ;
#285 = CARTESIAN_POINT ( 'NONE',  ( 232.5999999999999375, -33.74062499938548143, 103.1828516163667899 ) ) ;
#286 = CARTESIAN_POINT ( 'NONE',  ( -79.39999999999999147, -31.52268749875867471, 99.99999999999998579 ) ) ;
#287 = EDGE_LOOP ( 'NONE', ( #12680, #18333, #2040 ) ) ;
#288 = CARTESIAN_POINT ( 'NONE',  ( -82.39999999999999147, -33.74062499938548854, 103.1828516163667899 ) ) ;
#289 = CONICAL_SURFACE ( 'NONE', #10266, 4.000000000000000000, 0.8911886515913786111 ) ;
#290 = EDGE_CURVE ( 'NONE', #8383, #14066, #13875, .T. ) ;
#291 = CARTESIAN_POINT ( 'NONE',  ( -79.64356964374998427, -34.00312499938548427, -98.40857419181659793 ) ) ;
#292 = CARTESIAN_POINT ( 'NONE',  ( 82.39999999999999147, -34.30312499938548143, 103.1828516163667899 ) ) ;
#293 = CARTESIAN_POINT ( 'NONE',  ( 79.39999999999999147, -34.31250000000000000, 98.26794919243113213 ) ) ;
#294 =( BOUNDED_CURVE ( )  B_SPLINE_CURVE ( 2, ( #4333, #5428, #17722, #10192, #1107, #14385, #5519, #1310, #7258 ),
 .UNSPECIFIED., .F., .F. ) 
 B_SPLINE_CURVE_WITH_KNOTS ( ( 3, 2, 2, 2, 3 ),
 ( 0.3125000000000001665, 0.3194444444444444198, 0.3333333333333333148, 0.3472222222222222099, 0.3541666666666666297 ),
 .UNSPECIFIED. ) 
 CURVE ( )  GEOMETRIC_REPRESENTATION_ITEM ( )  RATIONAL_B_SPLINE_CURVE ( ( 0.9330127018922194093, 0.9330127018922209636, 1.000000000000000000, 0.8660254037844387076, 1.000000000000000000, 0.8660254037844387076, 1.000000000000000000, 0.9330127018922196314, 0.9330127018922194093 ) ) 
 REPRESENTATION_ITEM ( '' )  );
#295 = CARTESIAN_POINT ( 'NONE',  ( 110.9999999999999574, -21.80000000000003268, -142.6499999999999773 ) ) ;
#296 = CARTESIAN_POINT ( 'NONE',  ( 82.39999999999999147, -34.55624999877096570, -96.53589838486223584 ) ) ;
#297 = CARTESIAN_POINT ( 'NONE',  ( 234.0999999999999375, -34.35000000000000142, 102.5980762113533018 ) ) ;
#298 = ORIENTED_EDGE ( 'NONE', *, *, #2474, .F. ) ;
#299 = CARTESIAN_POINT ( 'NONE',  ( 235.3564303562499447, -34.04062499938548569, -51.59142580818350154 ) ) ;
#300 = CARTESIAN_POINT ( 'NONE',  ( 0.000000000000000000, 0.000000000000000000, 0.000000000000000000 ) ) ;
#301 = CARTESIAN_POINT ( 'NONE',  ( 232.5999999999999375, -31.04062499938547859, 103.1828516163667899 ) ) ;
#302 = CARTESIAN_POINT ( 'NONE',  ( 234.0999999999999375, -35.04374999877096286, -52.59807621135342970 ) ) ;
#303 = ADVANCED_FACE ( 'NONE', ( #13187 ), #10269, .F. ) ;
#304 = CARTESIAN_POINT ( 'NONE',  ( -85.15643035625001289, -35.05312499938548143, 101.5914258081833879 ) ) ;
#305 = ORIENTED_EDGE ( 'NONE', *, *, #12340, .T. ) ;
#306 = ORIENTED_EDGE ( 'NONE', *, *, #13225, .F. ) ;
#307 = CARTESIAN_POINT ( 'NONE',  ( 3.951447005078452701, -3.704664227300105583, 0.5833333333333329263 ) ) ;
#308 = CARTESIAN_POINT ( 'NONE',  ( -4.000000000000000000, 2.511478553582031203, -3.469254451724764543 ) ) ;
#309 = DIRECTION ( 'NONE',  ( -0.000000000000000000, -1.000000000000000000, -0.000000000000000000 ) ) ;
#310 = ORIENTED_EDGE ( 'NONE', *, *, #16679, .T. ) ;
#311 = CARTESIAN_POINT ( 'NONE',  ( -99.99999999999998579, -29.80000000000000426, 150.0000000000000000 ) ) ;
#312 = CARTESIAN_POINT ( 'NONE',  ( 229.5999999999999375, -34.03124999877096002, 98.26794919243111792 ) ) ;
#313 = DIRECTION ( 'NONE',  ( 1.000000000000000000, -1.387778780781445676E-15, -2.407412430484046130E-31 ) ) ;
#314 = CARTESIAN_POINT ( 'NONE',  ( -79.39999999999999147, -33.78750000000000142, 98.26794919243110371 ) ) ;
#315 = EDGE_CURVE ( 'NONE', #15577, #16231, #9273, .T. ) ;
#316 = CARTESIAN_POINT ( 'NONE',  ( -83.90000000000000568, -30.91874999877096997, 97.40192378864668399 ) ) ;
#317 = CARTESIAN_POINT ( 'NONE',  ( 235.2013144571816952, -32.00000000000002132, -51.47161334219405404 ) ) ;
#318 = ADVANCED_FACE ( 'NONE', ( #11630 ), #5967, .F. ) ;
#319 = CARTESIAN_POINT ( 'NONE',  ( -79.39999999999999147, -30.71250000000000213, 101.7320508075688537 ) ) ;
#320 = CARTESIAN_POINT ( 'NONE',  ( 82.40000000000000568, -34.61250000000001137, -97.00000000000000000 ) ) ;
#321 = CARTESIAN_POINT ( 'NONE',  ( -79.39999999999999147, -33.37500000000000000, 99.99999999999998579 ) ) ;
#322 = CARTESIAN_POINT ( 'NONE',  ( -82.40000000000000568, -30.00000000000000355, 103.0000000000000000 ) ) ;
#323 = EDGE_CURVE ( 'NONE', #14868, #14858, #1084, .T. ) ;
#324 = B_SPLINE_CURVE_WITH_KNOTS ( 'NONE', 3,
 ( #1017, #7159, #1300, #2555 ),
 .UNSPECIFIED., .F., .F.,
 ( 4, 4 ),
 ( 0.000000000000000000, 0.002080789711329297104 ),
 .UNSPECIFIED. ) ;
#325 = CARTESIAN_POINT ( 'NONE',  ( 229.8435696437499871, -32.42812499938548143, 98.40857419181659793 ) ) ;
#326 = ORIENTED_EDGE ( 'NONE', *, *, #4980, .F. ) ;
#327 = FILL_AREA_STYLE ('',( #7917 ) ) ;
#328 = CARTESIAN_POINT ( 'NONE',  ( -85.15643035624999868, -32.35312499938549280, -98.40857419181659793 ) ) ;
#329 = DIRECTION ( 'NONE',  ( -0.000000000000000000, -1.000000000000000000, -0.000000000000000000 ) ) ;
#330 = ORIENTED_EDGE ( 'NONE', *, *, #12340, .F. ) ;
#331 = DIRECTION ( 'NONE',  ( 1.000000000000000000, 0.000000000000000000, 0.000000000000000000 ) ) ;
#332 = CARTESIAN_POINT ( 'NONE',  ( 0.000000000000000000, 0.000000000000000000, 2.500000000000000444 ) ) ;
#333 = CARTESIAN_POINT ( 'NONE',  ( 231.5655627039840567, -35.00000000000000000, -47.42249611015796518 ) ) ;
#334 = CARTESIAN_POINT ( 'NONE',  ( 102.9999999999999858, -29.80000000000000071, -100.0000000000000000 ) ) ;
#335 = ORIENTED_EDGE ( 'NONE', *, *, #6417, .T. ) ;
#336 = EDGE_LOOP ( 'NONE', ( #9804, #7178, #6008, #18106, #9174, #4508, #17848 ) ) ;
#337 = CARTESIAN_POINT ( 'NONE',  ( 79.39999999999999147, -34.63124999877096855, 101.7320508075688963 ) ) ;
#338 = EDGE_CURVE ( 'NONE', #8719, #3780, #14563, .T. ) ;
#339 = CARTESIAN_POINT ( 'NONE',  ( 82.39999999999999147, -34.97812499938547859, -103.1828516163667899 ) ) ;
#340 = CARTESIAN_POINT ( 'NONE',  ( -79.39999999999999147, -31.03124999877097068, 98.26794919243110371 ) ) ;
#341 = CARTESIAN_POINT ( 'NONE',  ( 85.40000000000000568, -32.25000000000000000, 99.99999999999998579 ) ) ;
#342 = CARTESIAN_POINT ( 'NONE',  ( -83.52979456739218733, -32.00000000000002132, -97.41965524898077433 ) ) ;
#343 = CARTESIAN_POINT ( 'NONE',  ( 229.8435696437499871, -33.77812499938548285, 98.40857419181659793 ) ) ;
#344 = CARTESIAN_POINT ( 'NONE',  ( 83.77821517812500929, -32.42812499938548854, -102.3871387122750889 ) ) ;
#345 = CARTESIAN_POINT ( 'NONE',  ( 82.40000000000000568, -30.00000000000000355, 99.99999999999998579 ) ) ;
#346 = CARTESIAN_POINT ( 'NONE',  ( 85.15643035624999868, -33.32812499938548001, -98.40857419181659793 ) ) ;
#347 = ORIENTED_EDGE ( 'NONE', *, *, #19285, .F. ) ;
#348 = CARTESIAN_POINT ( 'NONE',  ( 235.5999999999999943, -33.78749999999999432, -51.73205080756900287 ) ) ;
#349 = ADVANCED_FACE ( 'NONE', ( #13762 ), #13787, .T. ) ;
#350 = CARTESIAN_POINT ( 'NONE',  ( -83.20384757729335945, -34.14240381056767148, 96.99999999999998579 ) ) ;
#351 = CARTESIAN_POINT ( 'NONE',  ( -85.40000000000000568, -34.08749999999999858, 98.26794919243111792 ) ) ;
#352 = DIRECTION ( 'NONE',  ( 0.000000000000000000, -1.000000000000000000, 0.000000000000000000 ) ) ;
#353 = CARTESIAN_POINT ( 'NONE',  ( -83.77821517812500929, -30.32812499938548711, 97.61286128772489690 ) ) ;
#354 = CARTESIAN_POINT ( 'NONE',  ( 235.3564303562499447, -33.14062499938548001, -51.59142580818350865 ) ) ;
#355 = CARTESIAN_POINT ( 'NONE',  ( -85.15643035624999868, -34.60312499938548569, 101.5914258081833879 ) ) ;
#356 = ORIENTED_EDGE ( 'NONE', *, *, #12713, .T. ) ;
#357 = CARTESIAN_POINT ( 'NONE',  ( -79.76502430829106061, -35.00019033771674515, 98.52379045060148144 ) ) ;
#358 = CARTESIAN_POINT ( 'NONE',  ( 232.5999999999999943, -34.30312499938547433, 96.81714838363319586 ) ) ;
#359 = CARTESIAN_POINT ( 'NONE',  ( 83.77821517812500929, -31.11562499938548498, 102.3871387122750889 ) ) ;
#360 = CARTESIAN_POINT ( 'NONE',  ( 235.5999999999999943, -34.76249999999999574, 101.7320508075688537 ) ) ;
#361 = CARTESIAN_POINT ( 'NONE',  ( -83.77821517812500929, -31.07812499938548711, 102.3871387122750889 ) ) ;
#362 = CARTESIAN_POINT ( 'NONE',  ( 235.5999999999999375, -32.01330983656912821, 99.46005447970520663 ) ) ;
#363 = CARTESIAN_POINT ( 'NONE',  ( 79.64356964374999848, -30.81562499938548427, 99.99999999999998579 ) ) ;
#364 = CARTESIAN_POINT ( 'NONE',  ( 83.77821517812500929, -32.57812499938548711, -97.61286128772489690 ) ) ;
#365 = CARTESIAN_POINT ( 'NONE',  ( 229.8435696437499303, -30.59062499938547575, -50.00000000000011369 ) ) ;
#366 = CARTESIAN_POINT ( 'NONE',  ( -84.67508262029694777, -32.00000000000000711, -98.43364869553373353 ) ) ;
#367 = CARTESIAN_POINT ( 'NONE',  ( -82.39999999999999147, -33.74062499938548854, -96.81714838363319586 ) ) ;
#368 = ORIENTED_EDGE ( 'NONE', *, *, #16035, .T. ) ;
#369 = CARTESIAN_POINT ( 'NONE',  ( 80.90000000000000568, -34.59374999877096712, 102.5980762113533018 ) ) ;
#370 = CARTESIAN_POINT ( 'NONE',  ( 232.5999999999999091, -34.38749999999999574, 102.9999999999999858 ) ) ;
#371 = CARTESIAN_POINT ( 'NONE',  ( -85.40000000000000568, -33.18750000000000000, 98.26794919243111792 ) ) ;
#372 = CARTESIAN_POINT ( 'NONE',  ( -83.77821517812500929, -34.37812499938548427, 97.61286128772489690 ) ) ;
#373 = CARTESIAN_POINT ( 'NONE',  ( 118.5000000000000284, 12.69999999999998508, 50.00000000000001421 ) ) ;
#374 = ORIENTED_EDGE ( 'NONE', *, *, #7762, .F. ) ;
#375 = CARTESIAN_POINT ( 'NONE',  ( -83.90000000000000568, -30.52500000000000213, -102.5980762113533018 ) ) ;
#376 = CARTESIAN_POINT ( 'NONE',  ( 83.04276107155152431, -34.99999999999999289, 102.9375709370400642 ) ) ;
#377 = CARTESIAN_POINT ( 'NONE',  ( 80.08630547029493130, -32.02340763552834346, -102.1282894555899361 ) ) ;
#378 = FACE_OUTER_BOUND ( 'NONE', #12586, .T. ) ;
#379 = CARTESIAN_POINT ( 'NONE',  ( 235.3564303562499447, -34.97812499938547859, 99.99999999999998579 ) ) ;
#380 = CARTESIAN_POINT ( 'NONE',  ( -80.90000000000000568, -35.19768749875867542, 102.5980762113533018 ) ) ;
#381 = EDGE_LOOP ( 'NONE', ( #16724, #7367, #9403, #6838, #9257, #5214, #15859, #12633, #9758, #10396, #17402, #15523, #2220, #3836, #18473, #563, #7521 ) ) ;
#382 = DIRECTION ( 'NONE',  ( -1.000000000000000000, 1.387778780781445676E-15, 2.407412430484046130E-31 ) ) ;
#383 = LINE ( 'NONE', #15609, #4157 ) ;
#384 = CARTESIAN_POINT ( 'NONE',  ( 79.64356964374998427, -32.57812499938548711, 101.5914258081833879 ) ) ;
#385 = CARTESIAN_POINT ( 'NONE',  ( 232.5999999999999375, -29.99999999999999645, -47.00000000000010658 ) ) ;
#386 = FACE_OUTER_BOUND ( 'NONE', #3807, .T. ) ;
#387 = CARTESIAN_POINT ( 'NONE',  ( 83.90000000000000568, -34.51874999877097139, -97.40192378864668399 ) ) ;
#388 = CYLINDRICAL_SURFACE ( 'NONE', #13636, 3.000000000000002665 ) ;
#389 = AXIS2_PLACEMENT_3D ( 'NONE', #88, #5845, #13359 ) ;
#390 = VECTOR ( 'NONE', #16629, 1000.000000000000000 ) ;
#391 = ORIENTED_EDGE ( 'NONE', *, *, #17376, .F. ) ;
#392 = CARTESIAN_POINT ( 'NONE',  ( 235.3564303562499447, -32.27812499938548285, -50.00000000000011369 ) ) ;
#393 = CARTESIAN_POINT ( 'NONE',  ( 233.9782151781249411, -31.30312499938547788, 97.61286128772489690 ) ) ;
#394 = CARTESIAN_POINT ( 'NONE',  ( 229.8435696437499303, -30.25312499938548072, -50.00000000000011369 ) ) ;
#395 = CARTESIAN_POINT ( 'NONE',  ( -81.59615242270662350, -33.01740381056767148, -96.99999999999998579 ) ) ;
#396 = ORIENTED_EDGE ( 'NONE', *, *, #404, .T. ) ;
#397 = ORIENTED_EDGE ( 'NONE', *, *, #4624, .T. ) ;
#398 = CARTESIAN_POINT ( 'NONE',  ( 4.211140560182196957, 2.431303136016536470, -3.745885042887433514 ) ) ;
#399 = CARTESIAN_POINT ( 'NONE',  ( -81.59615242270665192, -33.86115380933864571, -97.00000000000000000 ) ) ;
#400 = DIRECTION ( 'NONE',  ( 0.000000000000000000, 0.000000000000000000, 1.000000000000000000 ) ) ;
#401 = ORIENTED_EDGE ( 'NONE', *, *, #14601, .T. ) ;
#402 = CARTESIAN_POINT ( 'NONE',  ( 85.15643035625001289, -32.09062499938548996, 101.5914258081833879 ) ) ;
#403 = CARTESIAN_POINT ( 'NONE',  ( -80.90000000000000568, -32.79374999877096997, -102.5980762113533018 ) ) ;
#404 = EDGE_CURVE ( 'NONE', #11560, #13270, #807, .T. ) ;
#405 = AXIS2_PLACEMENT_3D ( 'NONE', #11450, #17508, #17414 ) ;
#406 = SHAPE_REPRESENTATION ( 'workbench', ( #10540 ), #11151 ) ;
#407 = AXIS2_PLACEMENT_3D ( 'NONE', #8734, #12848, #1036 ) ;
#408 = CARTESIAN_POINT ( 'NONE',  ( -82.40000000000000568, -33.93750000000000711, 102.9999999999999858 ) ) ;
#409 = CARTESIAN_POINT ( 'NONE',  ( -82.39999999999999147, -30.95624999877097139, 96.53589838486223584 ) ) ;
#410 = CARTESIAN_POINT ( 'NONE',  ( -80.90000000000000568, -34.14374999877097139, 97.40192378864668399 ) ) ;
#411 = CARTESIAN_POINT ( 'NONE',  ( 85.10336890118310293, -34.99999999999999289, -100.9939266215710347 ) ) ;
#412 = EDGE_CURVE ( 'NONE', #3766, #15452, #4691, .T. ) ;
#413 = EDGE_CURVE ( 'NONE', #18033, #12559, #12529, .T. ) ;
#414 = CARTESIAN_POINT ( 'NONE',  ( -85.15643035625001289, -35.22676544108147567, 98.99674642581742035 ) ) ;
#415 = PRESENTATION_STYLE_ASSIGNMENT (( #15246 ) ) ;
#416 = CARTESIAN_POINT ( 'NONE',  ( 232.5999999999999375, -34.97812499938547859, 103.1828516163667899 ) ) ;
#417 = CARTESIAN_POINT ( 'NONE',  ( 235.3564303562499447, -31.75312499938547717, 101.5914258081833879 ) ) ;
#418 = ORIENTED_EDGE ( 'NONE', *, *, #10898, .T. ) ;
#419 = CARTESIAN_POINT ( 'NONE',  ( -82.39999999999999147, -33.85312499938547859, -103.1828516163667899 ) ) ;
#420 = CARTESIAN_POINT ( 'NONE',  ( 4.158413352280809328, 4.089743253945649748, -5.087477719935601147E-16 ) ) ;
#421 = AXIS2_PLACEMENT_3D ( 'NONE', #13678, #16422, #3033 ) ;
#422 = VERTEX_POINT ( 'NONE', #7616 ) ;
#423 = AXIS2_PLACEMENT_3D ( 'NONE', #249, #13325, #17925 ) ;
#424 = CYLINDRICAL_SURFACE ( 'NONE', #15195, 5.200000000000009948 ) ;
#425 = CARTESIAN_POINT ( 'NONE',  ( 2.000000000000005329, -3.464101615137751722, 0.000000000000000000 ) ) ;
#426 = CARTESIAN_POINT ( 'NONE',  ( 230.1446115142513804, -34.99999999999998579, -51.72243138600839529 ) ) ;
#427 = ORIENTED_EDGE ( 'NONE', *, *, #13335, .T. ) ;
#428 = CARTESIAN_POINT ( 'NONE',  ( -82.40000000000000568, -30.00000000000000355, 99.99999999999998579 ) ) ;
#430 = EDGE_CURVE ( 'NONE', #19181, #5168, #15901, .T. ) ;
#429 = ORIENTED_EDGE ( 'NONE', *, *, #4800, .F. ) ;
#431 = ORIENTED_EDGE ( 'NONE', *, *, #17842, .F. ) ;
#432 = CARTESIAN_POINT ( 'NONE',  ( 233.4038475772933339, -33.28259618943232567, -53.00000000000011369 ) ) ;
#433 = CARTESIAN_POINT ( 'NONE',  ( 82.39999999999999147, -30.78750000000000497, -103.4641016151377499 ) ) ;
#434 = ADVANCED_FACE ( 'NONE', ( #18369 ), #12304, .F. ) ;
#435 = CARTESIAN_POINT ( 'NONE',  ( -79.39999999999999147, -34.21874999877096712, 99.99999999999998579 ) ) ;
#436 = CARTESIAN_POINT ( 'NONE',  ( -85.40000000000000568, -32.15624999877096712, -98.26794919243111792 ) ) ;
#438 = LINE ( 'NONE', #9597, #5397 ) ;
#437 = AXIS2_PLACEMENT_3D ( 'NONE', #16344, #19283, #7543 ) ;
#439 = CARTESIAN_POINT ( 'NONE',  ( 81.02178482187500208, -34.00312499938548427, -97.61286128772489690 ) ) ;
#440 = CARTESIAN_POINT ( 'NONE',  ( 85.15643035624999868, -34.22812499938547859, -98.40857419181659793 ) ) ;
#441 = ORIENTED_EDGE ( 'NONE', *, *, #8685, .F. ) ;
#442 = CARTESIAN_POINT ( 'NONE',  ( 231.0999999999999375, -33.07499999999999574, -47.40192378864679768 ) ) ;
#443 = CARTESIAN_POINT ( 'NONE',  ( -83.90000000000000568, -33.97500000000000853, 102.5980762113533018 ) ) ;
#444 = DIRECTION ( 'NONE',  ( 0.5000000000000015543, 0.8660254037844378194, 0.000000000000000000 ) ) ;
#445 = CARTESIAN_POINT ( 'NONE',  ( 230.2961164517930968, -35.00002705695767702, -51.92148140967023551 ) ) ;
#446 = CARTESIAN_POINT ( 'NONE',  ( -79.64356964375001269, -32.24062499938548854, 98.40857419181659793 ) ) ;
#447 = CARTESIAN_POINT ( 'NONE',  ( 232.5999999999999375, -33.29062499938547859, -46.81714838363331666 ) ) ;
#448 = CARTESIAN_POINT ( 'NONE',  ( -85.40000000000000568, -31.80000000000000071, 99.99999999999998579 ) ) ;
#449 = EDGE_LOOP ( 'NONE', ( #736, #12388, #396, #15662 ) ) ;
#450 = CARTESIAN_POINT ( 'NONE',  ( -84.70833260042415702, -35.00006955123599539, 98.08383195543535749 ) ) ;
#451 = FACE_OUTER_BOUND ( 'NONE', #8763, .T. ) ;
#452 = DIRECTION ( 'NONE',  ( 0.000000000000000000, 1.000000000000000000, 0.000000000000000000 ) ) ;
#453 = CARTESIAN_POINT ( 'NONE',  ( 84.74067385206575409, -31.99999999999999289, -98.53339280468588868 ) ) ;
#454 = CARTESIAN_POINT ( 'NONE',  ( -83.77821517812500929, -30.62812499938548783, 102.3871387122750889 ) ) ;
#455 = CARTESIAN_POINT ( 'NONE',  ( -82.39999999999999147, -32.16562499938548569, -103.1828516163667899 ) ) ;
#456 = CARTESIAN_POINT ( 'NONE',  ( 82.39999999999999147, -35.09062499938548285, 96.81714838363319586 ) ) ;
#457 = CARTESIAN_POINT ( 'NONE',  ( 81.02178482187500208, -30.85312499938548569, -97.61286128772489690 ) ) ;
#458 = EDGE_CURVE ( 'NONE', #16633, #11798, #16899, .T. ) ;
#459 = CARTESIAN_POINT ( 'NONE',  ( 229.8435696437499871, -31.90312499938547575, -48.40857419181671162 ) ) ;
#460 = CARTESIAN_POINT ( 'NONE',  ( -84.28136653320154892, -32.00000000000001421, 97.98546077809197641 ) ) ;
#461 = CARTESIAN_POINT ( 'NONE',  ( -79.64356964374999848, -33.17812499938548854, -99.99999999999998579 ) ) ;
#462 = ORIENTED_EDGE ( 'NONE', *, *, #14610, .T. ) ;
#463 = CARTESIAN_POINT ( 'NONE',  ( 85.15643035624999868, -33.81562499938549138, 98.40857419181659793 ) ) ;
#464 = FACE_OUTER_BOUND ( 'NONE', #16767, .T. ) ;
#465 = CARTESIAN_POINT ( 'NONE',  ( 4.124214193018025831, -2.028338413290977194, -3.513185186763603696 ) ) ;
#466 = CARTESIAN_POINT ( 'NONE',  ( -83.77821517812500929, -35.12812499938548427, 102.3871387122750889 ) ) ;
#467 = DIRECTION ( 'NONE',  ( 0.000000000000000000, 0.000000000000000000, -1.000000000000000000 ) ) ;
#468 = ORIENTED_EDGE ( 'NONE', *, *, #17120, .F. ) ;
#469 = CARTESIAN_POINT ( 'NONE',  ( -85.40000000000000568, -30.90000000000000213, -99.99999999999998579 ) ) ;
#470 = CARTESIAN_POINT ( 'NONE',  ( 82.65333140691207348, -34.99995246259152992, 102.9892844631211943 ) ) ;
#471 = CARTESIAN_POINT ( 'NONE',  ( 231.7960411235079050, -35.00000000000002132, -47.36341917746382535 ) ) ;
#472 = DIRECTION ( 'NONE',  ( 0.000000000000000000, -1.000000000000000000, 0.000000000000000000 ) ) ;
#473 = CARTESIAN_POINT ( 'NONE',  ( 231.7961524227065695, -33.00134618820329990, -47.00000000000011369 ) ) ;
#474 = CARTESIAN_POINT ( 'NONE',  ( 230.4884518427504076, -35.25364861271050643, 98.22820072003833047 ) ) ;
#475 = CARTESIAN_POINT ( 'NONE',  ( -85.40000000000000568, -34.03518749875867400, 98.26794919243111792 ) ) ;
#476 = ORIENTED_EDGE ( 'NONE', *, *, #19168, .T. ) ;
#477 = DIRECTION ( 'NONE',  ( -2.775557561562891351E-15, -1.000000000000000000, 0.000000000000000000 ) ) ;
#478 = CARTESIAN_POINT ( 'NONE',  ( 83.90000000000000568, -34.57500000000000284, -97.40192378864668399 ) ) ;
#479 = CARTESIAN_POINT ( 'NONE',  ( 79.64356964374999848, -34.86562499938548143, 99.99999999999998579 ) ) ;
#480 = CARTESIAN_POINT ( 'NONE',  ( 80.90000000000000568, -34.35000000000000853, 97.40192378864668399 ) ) ;
#481 = CARTESIAN_POINT ( 'NONE',  ( -83.20384757729337366, -34.35134618820330843, 103.0000000000000000 ) ) ;
#482 = CARTESIAN_POINT ( 'NONE',  ( 85.15643035624999868, -31.11562499938548854, -101.5914258081833879 ) ) ;
#483 = DIRECTION ( 'NONE',  ( 0.000000000000000000, -1.000000000000000000, 0.000000000000000000 ) ) ;
#484 = VERTEX_POINT ( 'NONE', #207 ) ;
#485 = CARTESIAN_POINT ( 'NONE',  ( 235.3564303562499447, -32.76562499938548001, -48.40857419181671162 ) ) ;
#486 = CARTESIAN_POINT ( 'NONE',  ( 231.2217848218749339, -32.42812499938548143, 102.3871387122750889 ) ) ;
#487 = CARTESIAN_POINT ( 'NONE',  ( 229.8435696437499871, -31.56562499938547717, -48.40857419181671162 ) ) ;
#488 = CARTESIAN_POINT ( 'NONE',  ( -82.39999999999999147, -33.85312499938547859, 96.81714838363319586 ) ) ;
#489 = CARTESIAN_POINT ( 'NONE',  ( 110.0000000000000142, 20.19999999999997797, -140.0000000000000000 ) ) ;
#490 = ORIENTED_EDGE ( 'NONE', *, *, #9846, .F. ) ;
#491 = ORIENTED_EDGE ( 'NONE', *, *, #16294, .F. ) ;
#492 = CARTESIAN_POINT ( 'NONE',  ( 4.175326769692870421, 2.060699556488908346, -3.569236330973472260 ) ) ;
#493 = CARTESIAN_POINT ( 'NONE',  ( -80.90000000000000568, -34.64999999999999858, 97.40192378864668399 ) ) ;
#494 = ORIENTED_EDGE ( 'NONE', *, *, #11033, .F. ) ;
#495 = CARTESIAN_POINT ( 'NONE',  ( 105.1999999999999886, -29.80000000000001492, -97.80000000000002558 ) ) ;
#496 = EDGE_CURVE ( 'NONE', #14858, #13499, #17905, .T. ) ;
#497 = CARTESIAN_POINT ( 'NONE',  ( -79.39999999999999147, -34.63124999877096855, -101.7320508075688821 ) ) ;
#498 = MECHANICAL_DESIGN_GEOMETRIC_PRESENTATION_REPRESENTATION (  '', ( #12637 ), #1099 ) ;
#499 = CARTESIAN_POINT ( 'NONE',  ( -4.000000000000000000, -2.309401076758515803, -0.4999999999999995559 ) ) ;
#500 = CARTESIAN_POINT ( 'NONE',  ( -82.39999999999999147, -31.40624999877097068, 96.53589838486223584 ) ) ;
#501 = CARTESIAN_POINT ( 'NONE',  ( -82.39999999999999147, -33.20624999877097139, 96.53589838486223584 ) ) ;
#502 = CARTESIAN_POINT ( 'NONE',  ( -82.40000000000000568, -30.50624999877097210, 96.99999999999998579 ) ) ;
#503 = CARTESIAN_POINT ( 'NONE',  ( 233.4038475772933623, -32.32634618820329564, 97.00000000000000000 ) ) ;
#504 = LINE ( 'NONE', #18569, #3508 ) ;
#505 = CARTESIAN_POINT ( 'NONE',  ( 235.3140393761304665, -32.00000000000000000, 101.2782762865722361 ) ) ;
#506 = CARTESIAN_POINT ( 'NONE',  ( 235.3564303562499447, -34.45312499938548001, 101.5914258081833879 ) ) ;
#507 = ORIENTED_EDGE ( 'NONE', *, *, #14382, .T. ) ;
#508 = CARTESIAN_POINT ( 'NONE',  ( 235.5999999999999943, -30.58124999877096073, 98.26794919243110371 ) ) ;
#509 = ORIENTED_EDGE ( 'NONE', *, *, #9352, .F. ) ;
#510 = AXIS2_PLACEMENT_3D ( 'NONE', #5921, #13234, #11867 ) ;
#511 = CARTESIAN_POINT ( 'NONE',  ( 4.197393957002303999, 7.772902908466098641E-14, -3.503767560748929810 ) ) ;
#512 = FACE_OUTER_BOUND ( 'NONE', #17537, .T. ) ;
#513 = CARTESIAN_POINT ( 'NONE',  ( 229.7512376763150996, -35.00000000000002842, -49.45334139305044374 ) ) ;
#514 = ORIENTED_EDGE ( 'NONE', *, *, #17717, .T. ) ;
#515 = DIRECTION ( 'NONE',  ( 0.000000000000000000, 0.000000000000000000, 1.000000000000000000 ) ) ;
#516 = EDGE_CURVE ( 'NONE', #5045, #540, #9364, .T. ) ;
#517 = ORIENTED_EDGE ( 'NONE', *, *, #5469, .F. ) ;
#518 = VERTEX_POINT ( 'NONE', #596 ) ;
#519 = DIRECTION ( 'NONE',  ( 0.000000000000000000, 0.000000000000000000, 1.000000000000000000 ) ) ;
#520 = CARTESIAN_POINT ( 'NONE',  ( 82.39999999999999147, -31.46250000000000568, -96.53589838486223584 ) ) ;
#521 = CARTESIAN_POINT ( 'NONE',  ( -85.40000000000000568, -30.39374999877097139, 99.99999999999998579 ) ) ;
#522 = CARTESIAN_POINT ( 'NONE',  ( -79.39999999999999147, -34.70624999877097139, 101.7320508075688537 ) ) ;
#523 = DIRECTION ( 'NONE',  ( 0.000000000000000000, -1.224646799147353947E-16, 1.000000000000000000 ) ) ;
#524 = CARTESIAN_POINT ( 'NONE',  ( 231.7961524227065979, -33.24240381056766580, 97.00000000000000000 ) ) ;
#525 = AXIS2_PLACEMENT_3D ( 'NONE', #5549, #9836, #16188 ) ;
#526 = CARTESIAN_POINT ( 'NONE',  ( 85.15643035625001289, -33.40312499938548285, -99.99999999999998579 ) ) ;
#527 = CARTESIAN_POINT ( 'NONE',  ( -83.77821517812500929, -33.81562499938548427, 97.61286128772489690 ) ) ;
#528 = EDGE_CURVE ( 'NONE', #3019, #11864, #4432, .T. ) ;
#529 = ADVANCED_FACE ( 'NONE', ( #15427 ), #2038, .T. ) ;
#530 = CARTESIAN_POINT ( 'NONE',  ( 82.39999999999999147, -32.72812499938548569, -103.1828516163667899 ) ) ;
#531 = VERTEX_POINT ( 'NONE', #18462 ) ;
#532 = CARTESIAN_POINT ( 'NONE',  ( 234.0999999999999375, -32.99999999999999289, -47.40192378864679768 ) ) ;
#533 =( LENGTH_UNIT ( ) NAMED_UNIT ( * ) SI_UNIT ( .MILLI., .METRE. ) );
#534 = CARTESIAN_POINT ( 'NONE',  ( 85.40000000000000568, -33.58124999877097139, -98.26794919243111792 ) ) ;
#535 = CARTESIAN_POINT ( 'NONE',  ( 233.9782151781249411, -32.20312499938548001, 97.61286128772489690 ) ) ;
#536 = CARTESIAN_POINT ( 'NONE',  ( -79.64356964375001269, -31.41562499938548569, 101.5914258081833879 ) ) ;
#537 = CARTESIAN_POINT ( 'NONE',  ( 233.9782151781249411, -33.55312499938548143, -52.38713871227520968 ) ) ;
#538 = CARTESIAN_POINT ( 'NONE',  ( -85.40000000000000568, -33.18750000000000000, 98.26794919243111792 ) ) ;
#539 = EDGE_CURVE ( 'NONE', #8610, #7775, #12491, .T. ) ;
#540 = VERTEX_POINT ( 'NONE', #17612 ) ;
#541 = CARTESIAN_POINT ( 'NONE',  ( 109.9999999999999574, -21.80000000000003268, -139.9999999999999716 ) ) ;
#542 = CARTESIAN_POINT ( 'NONE',  ( 235.5999999999999943, -33.86249999999999716, -48.26794919243124582 ) ) ;
#543 = CARTESIAN_POINT ( 'NONE',  ( 81.02178482187500208, -31.64062499938548356, 102.3871387122750889 ) ) ;
#544 = PRESENTATION_LAYER_ASSIGNMENT (  '', '', ( #8945 ) ) ;
#545 = CARTESIAN_POINT ( 'NONE',  ( 229.8848725447336960, -31.99999999999998579, -49.40473233008078324 ) ) ;
#546 = CARTESIAN_POINT ( 'NONE',  ( -83.77821517812500929, -32.57812499938548711, 97.61286128772489690 ) ) ;
#547 = AXIS2_PLACEMENT_3D ( 'NONE', #14828, #1559, #10535 ) ;
#548 = CARTESIAN_POINT ( 'NONE',  ( -82.39999999999999147, -32.39062499938548711, -96.81714838363319586 ) ) ;
#549 = CARTESIAN_POINT ( 'NONE',  ( 85.15643035624999868, -33.81562499938549138, 98.40857419181659793 ) ) ;
#550 = ADVANCED_FACE ( 'NONE', ( #16147 ), #10184, .T. ) ;
#551 = CARTESIAN_POINT ( 'NONE',  ( 79.64356964374999848, -31.37812499938548427, -99.99999999999998579 ) ) ;
#552 = CARTESIAN_POINT ( 'NONE',  ( 229.8435696437499303, -31.04062499938547859, -50.00000000000011369 ) ) ;
#553 = CARTESIAN_POINT ( 'NONE',  ( -82.39999999999999147, -34.41562499938548569, 96.81714838363319586 ) ) ;
#554 = CARTESIAN_POINT ( 'NONE',  ( -83.77821517812500929, -33.77812499938548285, -97.61286128772489690 ) ) ;
#555 = EDGE_CURVE ( 'NONE', #2812, #11515, #13893, .T. ) ;
#556 = ORIENTED_EDGE ( 'NONE', *, *, #12119, .F. ) ;
#557 = CARTESIAN_POINT ( 'NONE',  ( 79.64356964374999848, -32.27812499938548996, 99.99999999999998579 ) ) ;
#558 = AXIS2_PLACEMENT_3D ( 'NONE', #13780, #18191, #10944 ) ;
#559 = CARTESIAN_POINT ( 'NONE',  ( 3.880206590543188394, -2.665671387532522196, -2.382921720511056218 ) ) ;
#560 = CARTESIAN_POINT ( 'NONE',  ( -81.02178482187500208, -33.25312499938548427, 102.3871387122750889 ) ) ;
#561 =( BOUNDED_CURVE ( )  B_SPLINE_CURVE ( 2, ( #320, #6075, #16525, #7722, #13773, #6361, #4605, #12216, #218 ),
 .UNSPECIFIED., .F., .F. ) 
 B_SPLINE_CURVE_WITH_KNOTS ( ( 3, 2, 2, 2, 3 ),
 ( 0.8541666666666665186, 0.8611111111111111605, 0.8750000000000000000, 0.8888888888888888395, 0.8958333333333333703 ),
 .UNSPECIFIED. ) 
 CURVE ( )  GEOMETRIC_REPRESENTATION_ITEM ( )  RATIONAL_B_SPLINE_CURVE ( ( 0.9330127018922194093, 0.9330127018922177440, 1.000000000000000000, 0.8660254037844387076, 1.000000000000000000, 0.8660254037844387076, 1.000000000000000000, 0.9330127018922187432, 0.9330127018922192983 ) ) 
 REPRESENTATION_ITEM ( '' )  );
#562 = CARTESIAN_POINT ( 'NONE',  ( 233.4038475772933623, -32.11740381056766580, -47.00000000000011369 ) ) ;
#563 = ORIENTED_EDGE ( 'NONE', *, *, #2545, .T. ) ;
#564 = CARTESIAN_POINT ( 'NONE',  ( -82.39999999999999147, -32.81250000000000000, -103.4641016151377499 ) ) ;
#565 = AXIS2_PLACEMENT_3D ( 'NONE', #10279, #11928, #5692 ) ;
#566 = CARTESIAN_POINT ( 'NONE',  ( 2.805705207896068476, -3.226868319750173075, -3.503898532754370354 ) ) ;
#567 = PLANE ( 'NONE',  #8899 ) ;
#568 = EDGE_CURVE ( 'NONE', #13520, #13807, #4419, .T. ) ;
#569 = CARTESIAN_POINT ( 'NONE',  ( -81.02178482187500208, -34.60312499938549280, -97.61286128772489690 ) ) ;
#570 = CARTESIAN_POINT ( 'NONE',  ( 232.5999999999999375, -33.29062499938547859, 103.1828516163667899 ) ) ;
#571 = CARTESIAN_POINT ( 'NONE',  ( -80.90000000000000568, -34.74768749875867968, 102.5980762113533018 ) ) ;
#572 = VECTOR ( 'NONE', #4858, 1000.000000000000000 ) ;
#573 = ORIENTED_EDGE ( 'NONE', *, *, #9703, .F. ) ;
#574 = LINE ( 'NONE', #7790, #4310 ) ;
#575 = CARTESIAN_POINT ( 'NONE',  ( -6.259644161404860030E-16, -4.618802153517027165, -5.000000000000000000 ) ) ;
#576 = CARTESIAN_POINT ( 'NONE',  ( -83.90000000000000568, -33.07500000000000284, 102.5980762113533018 ) ) ;
#577 = CARTESIAN_POINT ( 'NONE',  ( 105.5000000000000142, 12.69999999999998508, 110.0000000000000142 ) ) ;
#578 = DIRECTION ( 'NONE',  ( -0.000000000000000000, -1.000000000000000000, -0.000000000000000000 ) ) ;
#579 = CARTESIAN_POINT ( 'NONE',  ( 79.64356964375001269, -30.44062499938548783, -98.40857419181659793 ) ) ;
#580 = AXIS2_PLACEMENT_3D ( 'NONE', #9951, #8566, #14520 ) ;
#581 = CARTESIAN_POINT ( 'NONE',  ( 4.114405500665260895, 2.025575754679705298, 3.508400121684924766 ) ) ;
#582 = VECTOR ( 'NONE', #10959, 1000.000000000000227 ) ;
#583 = ORIENTED_EDGE ( 'NONE', *, *, #17120, .T. ) ;
#584 = CARTESIAN_POINT ( 'NONE',  ( 85.40000000000000568, -30.88124999877097210, 101.7320508075688679 ) ) ;
#585 = APPLICATION_PROTOCOL_DEFINITION ( 'draft international standard', 'automotive_design', 1998, #5707 ) ;
#586 = CARTESIAN_POINT ( 'NONE',  ( 231.2217848218749339, -33.32812499938548001, 102.3871387122750889 ) ) ;
#587 = ADVANCED_FACE ( 'NONE', ( #14472 ), #5613, .F. ) ;
#588 = CARTESIAN_POINT ( 'NONE',  ( 231.2217848218749339, -31.67812499938547788, -52.38713871227520968 ) ) ;
#589 = CARTESIAN_POINT ( 'NONE',  ( -83.77821517812500929, -32.31562499938548427, 102.3871387122750889 ) ) ;
#590 = CARTESIAN_POINT ( 'NONE',  ( -80.90000000000000568, -32.85000000000000142, -102.5980762113533018 ) ) ;
#591 = VECTOR ( 'NONE', #8640, 1000.000000000000000 ) ;
#592 = VERTEX_POINT ( 'NONE', #17809 ) ;
#593 = ORIENTED_EDGE ( 'NONE', *, *, #12880, .F. ) ;
#594 = CARTESIAN_POINT ( 'NONE',  ( -82.39999999999999147, -32.50312499938548427, -103.1828516163667899 ) ) ;
#595 = CARTESIAN_POINT ( 'NONE',  ( -82.40000000000001990, -33.26250000000000284, 97.00000000000000000 ) ) ;
#596 = CARTESIAN_POINT ( 'NONE',  ( 82.40000000000001990, -34.61250000000001137, 103.0000000000000000 ) ) ;
#597 = ORIENTED_EDGE ( 'NONE', *, *, #11394, .T. ) ;
#598 = CARTESIAN_POINT ( 'NONE',  ( -4.000000000000000000, 0.1981133338132459731, 2.096406544454392723E-17 ) ) ;
#599 = CARTESIAN_POINT ( 'NONE',  ( -83.90000000000000568, -34.96874999877096712, -102.5980762113533018 ) ) ;
#600 = CIRCLE ( 'NONE', #3071, 2.649999999999980371 ) ;
#601 = CARTESIAN_POINT ( 'NONE',  ( -82.40000000000001990, -32.13750000000000284, 103.0000000000000000 ) ) ;
#602 = CARTESIAN_POINT ( 'NONE',  ( -85.40000000000000568, -31.33124999877096428, 98.26794919243111792 ) ) ;
#603 =( BOUNDED_SURFACE ( )  B_SPLINE_SURFACE ( 1, 2, ( 
 ( #2430, #8389, #14340, #978, #12884, #7121, #7303, #17575, #16392, #7401, #1447, #14820, #3002, #13364, #4186, #11893, #2816, #8773, #17670, #14628, #14530, #4283, #2082, #13260, #11606, #5752, #8863, #13163, #19234, #19135, #5946, #4380, #1359, #11701, #13075, #14723, #17864, #7210, #2911, #2715, #10146, #4475, #10248, #10428, #16210, #8957, #19040, #16301, #5850, #11804, #14926, #8675, #1552, #1162, #5663, #17773, #16108, #10337, #1263, #18372, #17090, #6355, #11224, #11121, #403, #11027, #8104, #9668, #17189, #16990, #4992, #6549, #15628, #16902, #9367, #15723, #13856, #3506, #10935, #12307, #10836, #2234, #12494, #1945, #9564, #13766, #3793, #15530, #3701, #2042, #3602, #9760, #5174, #18465, #18660, #18273, #8200, #5084, #7905, #2146, #4891, #7811, #14057, #14151, #8002, #691, #16805, #785, #6644, #5278, #3415, #6740, #15329, #497, #6451, #12403, #12591, #9465, #12686, #18559, #15430, #13958, #599, #10246, #17668, #19039, #5662, #14626, #10050, #4281, #2518, #2329, #881, #3994, #19132 ),
 ( #13161, #977, #11517, #13074, #7120, #10144, #9858, #8574, #14242, #5571, #17288, #5750, #4185, #17574, #11605, #11699, #16106, #11323, #8673, #1066, #7023, #9959, #6932, #8292, #15913, #2714, #18947, #18756, #11419, #1261, #12881, #17479, #18853, #7208, #2613, #12976, #17380, #6843, #14432, #12787, #5474, #5375, #15820, #3891, #2429, #8475, #8388, #4088, #14339, #16008, #1161, #14528, #1550, #13545, #16299, #13642, #185, #6136, #5848, #12086, #8861, #11891, #18060, #7499, #11802, #4378, #1444, #14818, #7593, #4671, #11990, #17958, #90, #6042, #7398, #12182, #17771, #13258, #4473, #13455, #13362, #3190, #2704, #2999, #10620, #16586, #5944, #10426, #4567, #10336, #10525, #9149, #16492, #16389, #2908, #283, #15112, #3095, #17862, #8955, #14924, #9055, #15020, #4772, #1640, #1727, #7685, #6234, #18150, #16208, #2814, #8770, #14721, #1357, #7301, #19232, #569, #3388, #9537, #12565, #15404, #1825, #18246, #760, #7879, #1916, #9438, #7785, #12282, #2211, #9340, #6524, #2118, #15503, #18533 ) ),
 .UNSPECIFIED., .F., .F., .F. ) 
 B_SPLINE_SURFACE_WITH_KNOTS ( ( 2, 2 ),
 ( 3, 2, 2, 2, 2, 2, 2, 2, 2, 2, 2, 2, 2, 2, 2, 2, 2, 2, 2, 2, 2, 2, 2, 2, 2, 2, 2, 2, 2, 2, 2, 2, 2, 2, 2, 2, 2, 2, 2, 2, 2, 2, 2, 2, 2, 2, 2, 2, 2, 2, 2, 2, 2, 2, 2, 2, 2, 2, 2, 2, 2, 2, 2, 2, 2, 2, 2, 3 ),
 ( 0.000000000000000000, 1.000000000000000000 ),
 ( 0.000000000000000000, 0.01388888888888888812, 0.02777777777777777624, 0.04166666666666666435, 0.05555555555555555247, 0.06944444444444444753, 0.08333333333333332871, 0.09722222222222222376, 0.1111111111111111049, 0.1250000000000000000, 0.1388888888888888951, 0.1527777777777777901, 0.1666666666666666574, 0.1805555555555555525, 0.1944444444444444475, 0.2083333333333333426, 0.2222222222222222099, 0.2361111111111111049, 0.2500000000000000000, 0.2638888888888888951, 0.2777777777777777901, 0.2916666666666666852, 0.3055555555555555802, 0.3194444444444444198, 0.3333333333333333148, 0.3472222222222222099, 0.3611111111111111049, 0.3750000000000000000, 0.3888888888888888951, 0.4027777777777777901, 0.4166666666666666852, 0.4305555555555555802, 0.4444444444444444198, 0.4583333333333333148, 0.4722222222222222099, 0.4861111111111111049, 0.5000000000000000000, 0.5138888888888888395, 0.5277777777777777901, 0.5416666666666666297, 0.5555555555555555802, 0.5694444444444444198, 0.5833333333333333703, 0.5972222222222222099, 0.6111111111111111605, 0.6250000000000000000, 0.6388888888888888395, 0.6527777777777777901, 0.6666666666666666297, 0.6805555555555555802, 0.6944444444444444198, 0.7083333333333333703, 0.7222222222222222099, 0.7361111111111111605, 0.7500000000000000000, 0.7638888888888888395, 0.7777777777777777901, 0.7916666666666666297, 0.8055555555555555802, 0.8194444444444444198, 0.8333333333333333703, 0.8472222222222222099, 0.8611111111111111605, 0.8750000000000000000, 0.8888888888888888395, 0.9027777777777777901, 0.9166666666666666297, 0.9258785144422092550 ),
 .UNSPECIFIED. ) 
 GEOMETRIC_REPRESENTATION_ITEM ( )  RATIONAL_B_SPLINE_SURFACE ( (
 ( 1.000000000000000000, 0.8660254037844387076, 1.000000000000000000, 0.8660254037844387076, 1.000000000000000000, 0.8660254037844387076, 1.000000000000000000, 0.8660254037844387076, 1.000000000000000000, 0.8660254037844387076, 1.000000000000000000, 0.8660254037844387076, 1.000000000000000000, 0.8660254037844387076, 1.000000000000000000, 0.8660254037844387076, 1.000000000000000000, 0.8660254037844387076, 1.000000000000000000, 0.8660254037844387076, 1.000000000000000000, 0.8660254037844387076, 1.000000000000000000, 0.8660254037844387076, 1.000000000000000000, 0.8660254037844387076, 1.000000000000000000, 0.8660254037844387076, 1.000000000000000000, 0.8660254037844387076, 1.000000000000000000, 0.8660254037844387076, 1.000000000000000000, 0.8660254037844387076, 1.000000000000000000, 0.8660254037844387076, 1.000000000000000000, 0.8660254037844387076, 1.000000000000000000, 0.8660254037844387076, 1.000000000000000000, 0.8660254037844387076, 1.000000000000000000, 0.8660254037844387076, 1.000000000000000000, 0.8660254037844387076, 1.000000000000000000, 0.8660254037844387076, 1.000000000000000000, 0.8660254037844387076, 1.000000000000000000, 0.8660254037844387076, 1.000000000000000000, 0.8660254037844387076, 1.000000000000000000, 0.8660254037844387076, 1.000000000000000000, 0.8660254037844387076, 1.000000000000000000, 0.8660254037844387076, 1.000000000000000000, 0.8660254037844387076, 1.000000000000000000, 0.8660254037844387076, 1.000000000000000000, 0.8660254037844387076, 1.000000000000000000, 0.8660254037844387076, 1.000000000000000000, 0.8660254037844387076, 1.000000000000000000, 0.8660254037844387076, 1.000000000000000000, 0.8660254037844387076, 1.000000000000000000, 0.8660254037844387076, 1.000000000000000000, 0.8660254037844387076, 1.000000000000000000, 0.8660254037844387076, 1.000000000000000000, 0.8660254037844387076, 1.000000000000000000, 0.8660254037844387076, 1.000000000000000000, 0.8660254037844387076, 1.000000000000000000, 0.8660254037844387076, 1.000000000000000000, 0.8660254037844387076, 1.000000000000000000, 0.8660254037844387076, 1.000000000000000000, 0.8660254037844387076, 1.000000000000000000, 0.8660254037844387076, 1.000000000000000000, 0.8660254037844387076, 1.000000000000000000, 0.8660254037844387076, 1.000000000000000000, 0.8660254037844387076, 1.000000000000000000, 0.8660254037844387076, 1.000000000000000000, 0.8660254037844387076, 1.000000000000000000, 0.8660254037844387076, 1.000000000000000000, 0.8660254037844387076, 1.000000000000000000, 0.8660254037844387076, 1.000000000000000000, 0.8660254037844387076, 1.000000000000000000, 0.8660254037844387076, 1.000000000000000000, 0.8660254037844387076, 1.000000000000000000, 0.8660254037844387076, 1.000000000000000000, 0.8660254037844387076, 1.000000000000000000, 0.8660254037844387076, 1.000000000000000000, 0.8660254037844387076, 1.000000000000000000, 0.8660254037844387076, 1.000000000000000000, 0.8660254037844387076, 1.000000000000000000, 0.8660254037844387076, 1.000000000000000000, 0.9111409417988175496, 0.9401539645359766606),
 ( 1.000000000000000000, 0.8660254037844387076, 1.000000000000000000, 0.8660254037844387076, 1.000000000000000000, 0.8660254037844387076, 1.000000000000000000, 0.8660254037844387076, 1.000000000000000000, 0.8660254037844387076, 1.000000000000000000, 0.8660254037844387076, 1.000000000000000000, 0.8660254037844387076, 1.000000000000000000, 0.8660254037844387076, 1.000000000000000000, 0.8660254037844387076, 1.000000000000000000, 0.8660254037844387076, 1.000000000000000000, 0.8660254037844387076, 1.000000000000000000, 0.8660254037844387076, 1.000000000000000000, 0.8660254037844387076, 1.000000000000000000, 0.8660254037844387076, 1.000000000000000000, 0.8660254037844387076, 1.000000000000000000, 0.8660254037844387076, 1.000000000000000000, 0.8660254037844387076, 1.000000000000000000, 0.8660254037844387076, 1.000000000000000000, 0.8660254037844387076, 1.000000000000000000, 0.8660254037844387076, 1.000000000000000000, 0.8660254037844387076, 1.000000000000000000, 0.8660254037844387076, 1.000000000000000000, 0.8660254037844387076, 1.000000000000000000, 0.8660254037844387076, 1.000000000000000000, 0.8660254037844387076, 1.000000000000000000, 0.8660254037844387076, 1.000000000000000000, 0.8660254037844387076, 1.000000000000000000, 0.8660254037844387076, 1.000000000000000000, 0.8660254037844387076, 1.000000000000000000, 0.8660254037844387076, 1.000000000000000000, 0.8660254037844387076, 1.000000000000000000, 0.8660254037844387076, 1.000000000000000000, 0.8660254037844387076, 1.000000000000000000, 0.8660254037844387076, 1.000000000000000000, 0.8660254037844387076, 1.000000000000000000, 0.8660254037844387076, 1.000000000000000000, 0.8660254037844387076, 1.000000000000000000, 0.8660254037844387076, 1.000000000000000000, 0.8660254037844387076, 1.000000000000000000, 0.8660254037844387076, 1.000000000000000000, 0.8660254037844387076, 1.000000000000000000, 0.8660254037844387076, 1.000000000000000000, 0.8660254037844387076, 1.000000000000000000, 0.8660254037844387076, 1.000000000000000000, 0.8660254037844387076, 1.000000000000000000, 0.8660254037844387076, 1.000000000000000000, 0.8660254037844387076, 1.000000000000000000, 0.8660254037844387076, 1.000000000000000000, 0.8660254037844387076, 1.000000000000000000, 0.8660254037844387076, 1.000000000000000000, 0.8660254037844387076, 1.000000000000000000, 0.8660254037844387076, 1.000000000000000000, 0.8660254037844387076, 1.000000000000000000, 0.8660254037844387076, 1.000000000000000000, 0.8660254037844387076, 1.000000000000000000, 0.8660254037844387076, 1.000000000000000000, 0.8660254037844387076, 1.000000000000000000, 0.8660254037844387076, 1.000000000000000000, 0.8660254037844387076, 1.000000000000000000, 0.8660254037844387076, 1.000000000000000000, 0.8660254037844387076, 1.000000000000000000, 0.8660254037844387076, 1.000000000000000000, 0.8660254037844387076, 1.000000000000000000, 0.8660254037844387076, 1.000000000000000000, 0.8660254037844387076, 1.000000000000000000, 0.8660254037844387076, 1.000000000000000000, 0.9111409417988175496, 0.9401539645359766606) ) ) 
 REPRESENTATION_ITEM ( '' )  SURFACE ( )  );
#604 = CARTESIAN_POINT ( 'NONE',  ( -79.39999999999999147, -35.11874999877096570, 99.99999999999998579 ) ) ;
#605 = DIRECTION ( 'NONE',  ( 0.000000000000000000, 0.000000000000000000, 1.000000000000000000 ) ) ;
#606 = CARTESIAN_POINT ( 'NONE',  ( 81.59615242270662350, -34.12634618820329990, -96.99999999999998579 ) ) ;
#607 = CARTESIAN_POINT ( 'NONE',  ( -82.40000000000000568, -30.50624999877097210, 96.99999999999998579 ) ) ;
#608 = CARTESIAN_POINT ( 'NONE',  ( 229.8435696437499303, -33.74062499938548143, 99.99999999999998579 ) ) ;
#609 = VERTEX_POINT ( 'NONE', #4327 ) ;
#610 = CARTESIAN_POINT ( 'NONE',  ( -79.64356964375001269, -34.82812499938548711, -101.5914258081833879 ) ) ;
#611 = CARTESIAN_POINT ( 'NONE',  ( 82.40000000000000568, -30.00000000000000355, -96.99999999999998579 ) ) ;
#612 = ORIENTED_EDGE ( 'NONE', *, *, #5825, .F. ) ;
#613 = CARTESIAN_POINT ( 'NONE',  ( -83.90000000000000568, -33.46874999877096712, 102.5980762113533018 ) ) ;
#614 = FACE_OUTER_BOUND ( 'NONE', #13488, .T. ) ;
#615 = UNCERTAINTY_MEASURE_WITH_UNIT (LENGTH_MEASURE( 1.000000000000000082E-05 ), #15735, 'distance_accuracy_value', 'NONE');
#616 = CYLINDRICAL_SURFACE ( 'NONE', #18162, 3.000000000000002665 ) ;
#617 = ORIENTED_EDGE ( 'NONE', *, *, #15683, .T. ) ;
#618 = CARTESIAN_POINT ( 'NONE',  ( 233.9782151781249411, -34.34062499938547575, -52.38713871227520968 ) ) ;
#619 = CARTESIAN_POINT ( 'NONE',  ( -81.59615242270665192, -33.86115380933864571, 103.0000000000000000 ) ) ;
#620 = ORIENTED_EDGE ( 'NONE', *, *, #7465, .T. ) ;
#621 = CARTESIAN_POINT ( 'NONE',  ( -84.44763168836716716, -32.00000000000000000, 101.8452947671445799 ) ) ;
#622 = CARTESIAN_POINT ( 'NONE',  ( 80.90000000000000568, -30.30000000000000426, -102.5980762113533018 ) ) ;
#623 = FACE_OUTER_BOUND ( 'NONE', #2442, .T. ) ;
#624 = CARTESIAN_POINT ( 'NONE',  ( -85.40000000000000568, -35.36739044046696279, 98.90809476984486537 ) ) ;
#625 = CARTESIAN_POINT ( 'NONE',  ( -79.39999999999999147, -33.82106250001229597, 99.99999999999998579 ) ) ;
#626 = CARTESIAN_POINT ( 'NONE',  ( 83.20384757729337366, -32.15759618943233278, -103.0000000000000000 ) ) ;
#627 = CARTESIAN_POINT ( 'NONE',  ( 229.5999999999999375, -33.14999999999999147, 99.99999999999998579 ) ) ;
#628 = CARTESIAN_POINT ( 'NONE',  ( 83.77821517812500929, -34.22812499938549280, -102.3871387122750889 ) ) ;
#629 = CARTESIAN_POINT ( 'NONE',  ( 235.2218879900010506, -35.00000000000000000, -49.14934632385183022 ) ) ;
#630 = CARTESIAN_POINT ( 'NONE',  ( -79.64356964375001269, -32.12812499938548427, 98.40857419181659793 ) ) ;
#631 = CARTESIAN_POINT ( 'NONE',  ( 79.64356964374999848, -33.96562499938548285, -99.99999999999998579 ) ) ;
#632 = EDGE_LOOP ( 'NONE', ( #11535, #18764, #13842, #12752 ) ) ;
#633 = CARTESIAN_POINT ( 'NONE',  ( 231.0999999999999375, -33.97500000000000142, -47.40192378864679768 ) ) ;
#634 = CARTESIAN_POINT ( 'NONE',  ( -80.90000000000000568, -33.89999999999999858, 102.5980762113533018 ) ) ;
#635 =( BOUNDED_CURVE ( )  B_SPLINE_CURVE ( 2, ( #15798, #17169, #11586, #14410, #9739, #11298, #14220, #11396, #15704 ),
 .UNSPECIFIED., .F., .F. ) 
 B_SPLINE_CURVE_WITH_KNOTS ( ( 3, 2, 2, 2, 3 ),
 ( 0.6458333333333333703, 0.6527777777777777901, 0.6666666666666666297, 0.6805555555555555802, 0.6875000000000000000 ),
 .UNSPECIFIED. ) 
 CURVE ( )  GEOMETRIC_REPRESENTATION_ITEM ( )  RATIONAL_B_SPLINE_CURVE ( ( 0.9330127018922192983, 0.9330127018922198534, 1.000000000000000000, 0.8660254037844387076, 1.000000000000000000, 0.8660254037844387076, 1.000000000000000000, 0.9330127018922194093, 0.9330127018922194093 ) ) 
 REPRESENTATION_ITEM ( '' )  );
#636 = CARTESIAN_POINT ( 'NONE',  ( -83.20384757729335945, -30.80759618943233846, 102.9999999999999858 ) ) ;
#637 = CARTESIAN_POINT ( 'NONE',  ( 232.5999999999999943, -32.84062499938548285, 103.1828516163667899 ) ) ;
#638 = CARTESIAN_POINT ( 'NONE',  ( -83.77821517812500929, -31.97812499938548925, 102.3871387122750889 ) ) ;
#639 = CARTESIAN_POINT ( 'NONE',  ( 235.3564303562499447, -33.59062499938548285, -51.59142580818350865 ) ) ;
#640 = CARTESIAN_POINT ( 'NONE',  ( -80.90000000000000568, -32.55000000000000426, 102.5980762113533018 ) ) ;
#641 = ORIENTED_EDGE ( 'NONE', *, *, #9035, .F. ) ;
#642 = CARTESIAN_POINT ( 'NONE',  ( 3.961557105775382670, -1.423285172353652817, 3.500000000000000444 ) ) ;
#643 = CARTESIAN_POINT ( 'NONE',  ( 232.5999999999999375, -33.93749999999999289, -47.00000000000011369 ) ) ;
#644 = CARTESIAN_POINT ( 'NONE',  ( 83.77821517812500929, -31.56562499938548427, 102.3871387122750889 ) ) ;
#645 = EDGE_CURVE ( 'NONE', #12702, #6637, #2949, .T. ) ;
#646 = CARTESIAN_POINT ( 'NONE',  ( 230.5871892821561175, -32.00000000000001421, -51.89178425775511272 ) ) ;
#647 = CARTESIAN_POINT ( 'NONE',  ( -81.02178482187500208, -31.30312499938548498, 97.61286128772489690 ) ) ;
#648 = CARTESIAN_POINT ( 'NONE',  ( -83.77821517812500929, -32.42812499938548854, -97.61286128772489690 ) ) ;
#649 = CARTESIAN_POINT ( 'NONE',  ( 79.64356964375001269, -32.12812499938548427, 101.5914258081833879 ) ) ;
#650 = ADVANCED_FACE ( 'NONE', ( #8903 ), #14768, .T. ) ;
#651 = CARTESIAN_POINT ( 'NONE',  ( 85.15643035624999868, -30.66562499938548569, -101.5914258081833879 ) ) ;
#652 = CARTESIAN_POINT ( 'NONE',  ( 235.3564303562499447, -31.26562499938547646, -50.00000000000011369 ) ) ;
#653 = CARTESIAN_POINT ( 'NONE',  ( -85.15643035625001289, -34.34062499938548285, 98.40857419181659793 ) ) ;
#654 = CARTESIAN_POINT ( 'NONE',  ( -81.02178482187500208, -32.80312499938548854, -97.61286128772489690 ) ) ;
#655 = ORIENTED_EDGE ( 'NONE', *, *, #15701, .F. ) ;
#656 = CARTESIAN_POINT ( 'NONE',  ( 81.02178482187500208, -32.80312499938548854, 97.61286128772489690 ) ) ;
#657 = CARTESIAN_POINT ( 'NONE',  ( 233.4038475772933054, -34.36740381056765870, 102.9999999999999858 ) ) ;
#658 = CARTESIAN_POINT ( 'NONE',  ( -79.64356964374999848, -30.36562499938548498, 99.99999999999998579 ) ) ;
#659 = CARTESIAN_POINT ( 'NONE',  ( -79.64356964374999848, -34.07812499938548711, 99.99999999999998579 ) ) ;
#660 = CARTESIAN_POINT ( 'NONE',  ( 235.5999999999999659, -32.01330983656912110, -50.53994552029475074 ) ) ;
#661 = EDGE_LOOP ( 'NONE', ( #10048, #2017, #17543, #5703 ) ) ;
#662 = CARTESIAN_POINT ( 'NONE',  ( -79.39999999999999147, -32.43750000000000000, -101.7320508075688821 ) ) ;
#663 = ADVANCED_FACE ( 'NONE', ( #13403 ), #5985, .F. ) ;
#664 = CARTESIAN_POINT ( 'NONE',  ( 0.000000000000000000, 0.000000000000000000, -5.000000000000000000 ) ) ;
#665 = CARTESIAN_POINT ( 'NONE',  ( -2.100000000000000089, 2.571758278209441957E-16, -4.694516984716113228 ) ) ;
#666 = DIRECTION ( 'NONE',  ( 0.000000000000000000, 0.000000000000000000, -1.000000000000000000 ) ) ;
#667 = ADVANCED_FACE ( 'NONE', ( #13111 ), #7348, .T. ) ;
#668 = CARTESIAN_POINT ( 'NONE',  ( 229.8435696437499303, -33.40312499938547575, 99.99999999999998579 ) ) ;
#669 = CARTESIAN_POINT ( 'NONE',  ( -79.39999999999999147, -34.71018749875867826, 101.7320508075688537 ) ) ;
#670 = ORIENTED_EDGE ( 'NONE', *, *, #8877, .T. ) ;
#671 = CARTESIAN_POINT ( 'NONE',  ( 82.40000000000000568, -30.00000000000000355, -99.99999999999998579 ) ) ;
#672 = DIRECTION ( 'NONE',  ( 0.8660254037844379305, 0.5000000000000013323, 0.000000000000000000 ) ) ;
#673 = DIRECTION ( 'NONE',  ( 1.000000000000000000, -1.387778780781445676E-15, -2.407412430484046130E-31 ) ) ;
#674 = DIRECTION ( 'NONE',  ( -0.000000000000000000, -0.000000000000000000, -1.000000000000000000 ) ) ;
#675 = CARTESIAN_POINT ( 'NONE',  ( 85.15643035625001289, -30.70312499938548711, -99.99999999999998579 ) ) ;
#676 = FACE_OUTER_BOUND ( 'NONE', #12537, .T. ) ;
#677 = VERTEX_POINT ( 'NONE', #10287 ) ;
#678 =( BOUNDED_CURVE ( )  B_SPLINE_CURVE ( 2, ( #4464, #17947, #13065, #17565, #8947, #19221, #11597, #8854, #5742 ),
 .UNSPECIFIED., .F., .F. ) 
 B_SPLINE_CURVE_WITH_KNOTS ( ( 3, 2, 2, 2, 3 ),
 ( 0.3958333333333334259, 0.4027777777777777901, 0.4166666666666666852, 0.4305555555555555802, 0.4374999999999999445 ),
 .UNSPECIFIED. ) 
 CURVE ( )  GEOMETRIC_REPRESENTATION_ITEM ( )  RATIONAL_B_SPLINE_CURVE ( ( 0.9330127018922192983, 0.9330127018922200755, 1.000000000000000000, 0.8660254037844387076, 1.000000000000000000, 0.8660254037844387076, 1.000000000000000000, 0.9330127018922198534, 0.9330127018922192983 ) ) 
 REPRESENTATION_ITEM ( '' )  );
#679 = CARTESIAN_POINT ( 'NONE',  ( 79.39999999999999147, -31.03124999877097068, 101.7320508075688821 ) ) ;
#680 = APPLICATION_PROTOCOL_DEFINITION ( 'draft international standard', 'automotive_design', 1998, #19198 ) ;
#681 = CARTESIAN_POINT ( 'NONE',  ( 235.3564303562499447, -33.17812499938548143, 99.99999999999998579 ) ) ;
#682 = CARTESIAN_POINT ( 'NONE',  ( 232.5999999999999375, -32.39062499938548001, -46.81714838363331666 ) ) ;
#683 = CARTESIAN_POINT ( 'NONE',  ( -83.77821517812500929, -34.56562499938548427, 102.3871387122750889 ) ) ;
#684 = CARTESIAN_POINT ( 'NONE',  ( -79.39999999999999147, -32.92500000000000426, -99.99999999999998579 ) ) ;
#685 = EDGE_LOOP ( 'NONE', ( #18840, #966, #7472, #17589 ) ) ;
#686 = ORIENTED_EDGE ( 'NONE', *, *, #7224, .F. ) ;
#687 = CARTESIAN_POINT ( 'NONE',  ( -85.15643035624999868, -31.07812499938548356, -101.5914258081833879 ) ) ;
#688 = CARTESIAN_POINT ( 'NONE',  ( -83.20384757729337366, -32.34240381056766722, -103.0000000000000000 ) ) ;
#689 = ORIENTED_EDGE ( 'NONE', *, *, #8646, .T. ) ;
#690 = CARTESIAN_POINT ( 'NONE',  ( 83.77821517812500929, -33.32812499938548711, 97.61286128772489690 ) ) ;
#691 = CARTESIAN_POINT ( 'NONE',  ( -82.39999999999999147, -34.33124999877097139, -96.53589838486223584 ) ) ;
#692 = CARTESIAN_POINT ( 'NONE',  ( 82.39999999999999147, -33.93750000000000000, 96.53589838486223584 ) ) ;
#693 = CARTESIAN_POINT ( 'NONE',  ( -79.39999999999999147, -34.31250000000000000, 101.7320508075688537 ) ) ;
#694 = CARTESIAN_POINT ( 'NONE',  ( -79.39999999999999147, -32.90624999877096712, 101.7320508075688537 ) ) ;
#695 = EDGE_CURVE ( 'NONE', #5463, #11282, #11271, .T. ) ;
#696 = CARTESIAN_POINT ( 'NONE',  ( -85.40000000000000568, -34.03124999877096712, 98.26794919243111792 ) ) ;
#697 = CARTESIAN_POINT ( 'NONE',  ( -83.90000000000000568, -32.17500000000000426, 102.5980762113533018 ) ) ;
#698 = CARTESIAN_POINT ( 'NONE',  ( 229.5999999999999375, -34.03124999877096002, -51.73205080756898866 ) ) ;
#699 = CARTESIAN_POINT ( 'NONE',  ( 83.90000000000000568, -30.46874999877096712, -97.40192378864668399 ) ) ;
#700 = CARTESIAN_POINT ( 'NONE',  ( 235.3564303562499447, -33.02812499938547575, 98.40857419181659793 ) ) ;
#701 = ORIENTED_EDGE ( 'NONE', *, *, #9112, .F. ) ;
#702 = CARTESIAN_POINT ( 'NONE',  ( 83.77821517812500929, -33.36562499938548854, -97.61286128772489690 ) ) ;
#703 =( LENGTH_UNIT ( ) NAMED_UNIT ( * ) SI_UNIT ( .MILLI., .METRE. ) );
#704 = EDGE_CURVE ( 'NONE', #8584, #4219, #13266, .T. ) ;
#705 = CARTESIAN_POINT ( 'NONE',  ( 229.5999999999999375, -31.25624999877096144, 101.7320508075688679 ) ) ;
#706 = LINE ( 'NONE', #16822, #18035 ) ;
#707 = ORIENTED_EDGE ( 'NONE', *, *, #14527, .F. ) ;
#708 = CARTESIAN_POINT ( 'NONE',  ( 82.40000000000000568, -30.00000000000000355, -103.0000000000000000 ) ) ;
#709 = CARTESIAN_POINT ( 'NONE',  ( 0.3208286057739604957, -4.433571671609698228, -0.3503314178412692548 ) ) ;
#710 = CARTESIAN_POINT ( 'NONE',  ( -82.40000000000000568, -35.00000000000000000, 99.99999999999998579 ) ) ;
#711 = VERTEX_POINT ( 'NONE', #7829 ) ;
#712 = CARTESIAN_POINT ( 'NONE',  ( -79.39999999999999147, -31.93124999877096926, 98.26794919243110371 ) ) ;
#713 = VECTOR ( 'NONE', #18943, 1000.000000000000000 ) ;
#714 = CARTESIAN_POINT ( 'NONE',  ( -82.40000000000001990, -33.88124999877096855, 103.0000000000000000 ) ) ;
#715 = EDGE_LOOP ( 'NONE', ( #13037, #16003, #5872 ) ) ;
#716 =( BOUNDED_CURVE ( )  B_SPLINE_CURVE ( 2, ( #8573, #10335, #8671, #13360, #14625, #1549, #11516, #4377, #5749 ),
 .UNSPECIFIED., .F., .F. ) 
 B_SPLINE_CURVE_WITH_KNOTS ( ( 3, 2, 2, 2, 3 ),
 ( 0.3125000000000001665, 0.3194444444444444198, 0.3333333333333333148, 0.3472222222222222099, 0.3541666666666666297 ),
 .UNSPECIFIED. ) 
 CURVE ( )  GEOMETRIC_REPRESENTATION_ITEM ( )  RATIONAL_B_SPLINE_CURVE ( ( 0.9330127018922194093, 0.9330127018922209636, 1.000000000000000000, 0.8660254037844387076, 1.000000000000000000, 0.8660254037844387076, 1.000000000000000000, 0.9330127018922196314, 0.9330127018922194093 ) ) 
 REPRESENTATION_ITEM ( '' )  );
#717 = CARTESIAN_POINT ( 'NONE',  ( 81.02178482187500208, -34.79062499938548569, -97.61286128772489690 ) ) ;
#718 = DIRECTION ( 'NONE',  ( -0.000000000000000000, -1.000000000000000000, -0.000000000000000000 ) ) ;
#719 = CARTESIAN_POINT ( 'NONE',  ( -83.90000000000000568, -33.91874999877096997, 102.5980762113533018 ) ) ;
#720 = CARTESIAN_POINT ( 'NONE',  ( -80.90000000000000568, -30.30000000000000426, 102.5980762113533018 ) ) ;
#721 = DIRECTION ( 'NONE',  ( -0.000000000000000000, -0.000000000000000000, -1.000000000000000000 ) ) ;
#722 = CARTESIAN_POINT ( 'NONE',  ( -3.680118525130244400, 2.494084732383327285, -0.3507732604232449702 ) ) ;
#723 = CARTESIAN_POINT ( 'NONE',  ( 79.64356964374999848, -32.16562499938548569, 99.99999999999998579 ) ) ;
#724 = DIRECTION ( 'NONE',  ( -0.000000000000000000, -1.000000000000000000, -0.000000000000000000 ) ) ;
#725 = CARTESIAN_POINT ( 'NONE',  ( -83.77821517812500929, -33.21562499938548285, 102.3871387122750889 ) ) ;
#726 = AXIS2_PLACEMENT_3D ( 'NONE', #3795, #17290, #18856 ) ;
#727 = AXIS2_PLACEMENT_3D ( 'NONE', #19099, #14307, #4057 ) ;
#728 = LINE ( 'NONE', #14088, #8969 ) ;
#729 = VERTEX_POINT ( 'NONE', #6372 ) ;
#730 = CARTESIAN_POINT ( 'NONE',  ( 229.5999999999999375, -34.01249999999999574, -48.26794919243123161 ) ) ;
#731 = CARTESIAN_POINT ( 'NONE',  ( -80.90000000000000568, -34.80000000000000426, 102.5980762113533018 ) ) ;
#732 = DIRECTION ( 'NONE',  ( 0.000000000000000000, 0.000000000000000000, -1.000000000000000000 ) ) ;
#733 = CARTESIAN_POINT ( 'NONE',  ( -82.39999999999999147, -33.06562499938548427, 96.81714838363319586 ) ) ;
#734 = CARTESIAN_POINT ( 'NONE',  ( 235.3564303562499447, -31.22812499938548214, -51.59142580818350865 ) ) ;
#735 = CARTESIAN_POINT ( 'NONE',  ( -79.39999999999999147, -32.88750000000000284, 98.26794919243110371 ) ) ;
#736 = ORIENTED_EDGE ( 'NONE', *, *, #13637, .F. ) ;
#737 = CARTESIAN_POINT ( 'NONE',  ( -82.32247963938036150, -35.00000000000000711, -97.23891671615864141 ) ) ;
#738 = CARTESIAN_POINT ( 'NONE',  ( 81.02178482187500208, -33.59062499938548285, 97.61286128772489690 ) ) ;
#739 = CARTESIAN_POINT ( 'NONE',  ( 85.40000000000000568, -32.60624999877096997, -101.7320508075688821 ) ) ;
#740 = CARTESIAN_POINT ( 'NONE',  ( -81.02178482187500208, -32.65312499938548996, 97.61286128772489690 ) ) ;
#741 = CARTESIAN_POINT ( 'NONE',  ( 83.52979456739228681, -32.00000000000000000, 97.41965524898084539 ) ) ;
#742 = CARTESIAN_POINT ( 'NONE',  ( 83.77821517812500929, -31.41562499938548569, 97.61286128772489690 ) ) ;
#743 =( BOUNDED_CURVE ( )  B_SPLINE_CURVE ( 2, ( #10018, #7083, #18723, #14593, #5344, #12754, #5443, #17347, #18913 ),
 .UNSPECIFIED., .F., .F. ) 
 B_SPLINE_CURVE_WITH_KNOTS ( ( 3, 2, 2, 2, 3 ),
 ( 0.6874999999999997780, 0.6944444444444444198, 0.7083333333333333703, 0.7222222222222222099, 0.7291666666666665186 ),
 .UNSPECIFIED. ) 
 CURVE ( )  GEOMETRIC_REPRESENTATION_ITEM ( )  RATIONAL_B_SPLINE_CURVE ( ( 0.9330127018922194093, 0.9330127018922171889, 1.000000000000000000, 0.8660254037844387076, 1.000000000000000000, 0.8660254037844387076, 1.000000000000000000, 0.9330127018922209636, 0.9330127018922194093 ) ) 
 REPRESENTATION_ITEM ( '' )  );
#744 = CARTESIAN_POINT ( 'NONE',  ( 85.15643035624999868, -32.54062499938548569, -98.40857419181659793 ) ) ;
#745 = CARTESIAN_POINT ( 'NONE',  ( 235.3564303562499447, -32.57812499938547290, -51.59142580818350865 ) ) ;
#746 = CARTESIAN_POINT ( 'NONE',  ( -82.39999999999999147, -33.51562499938548711, 96.81714838363319586 ) ) ;
#747 = CARTESIAN_POINT ( 'NONE',  ( -83.77821517812500929, -30.96562499938548640, -97.61286128772489690 ) ) ;
#748 = ORIENTED_EDGE ( 'NONE', *, *, #11145, .T. ) ;
#749 = CARTESIAN_POINT ( 'NONE',  ( 79.64356964374999848, -33.62812499938548427, 99.99999999999998579 ) ) ;
#750 = CARTESIAN_POINT ( 'NONE',  ( -83.20384757729335945, -33.00134618820329990, 102.9999999999999858 ) ) ;
#751 = CARTESIAN_POINT ( 'NONE',  ( -85.15643035624999868, -31.45312499938548356, 101.5914258081833879 ) ) ;
#752 = CARTESIAN_POINT ( 'NONE',  ( -85.15643035624999868, -34.34062499938548285, 98.40857419181659793 ) ) ;
#753 = CARTESIAN_POINT ( 'NONE',  ( 85.40000000000000568, -34.95000000000000284, 99.99999999999998579 ) ) ;
#754 = EDGE_LOOP ( 'NONE', ( #205, #16125, #13208, #6303 ) ) ;
#755 = CARTESIAN_POINT ( 'NONE',  ( -85.40000000000000568, -34.01250000000000284, -98.26794919243111792 ) ) ;
#756 = EDGE_CURVE ( 'NONE', #10068, #15900, #4525, .T. ) ;
#757 = EDGE_CURVE ( 'NONE', #1894, #5820, #10757, .T. ) ;
#758 = CARTESIAN_POINT ( 'NONE',  ( 4.211140560182196957, -2.431303136016555122, -3.745885042887436622 ) ) ;
#759 = CARTESIAN_POINT ( 'NONE',  ( 230.8788704469753839, -35.00000000000000000, -52.46580019096116132 ) ) ;
#760 = CARTESIAN_POINT ( 'NONE',  ( -82.39999999999999147, -34.86562499938548854, -103.1828516163667899 ) ) ;
#761 = CARTESIAN_POINT ( 'NONE',  ( 232.5999999999999375, -30.70312499938548001, 96.81714838363319586 ) ) ;
#762 = CARTESIAN_POINT ( 'NONE',  ( -79.39999999999999147, -33.36018749875868394, 101.7320508075688537 ) ) ;
#763 = CYLINDRICAL_SURFACE ( 'NONE', #16164, 3.000000000000002665 ) ;
#764 = CARTESIAN_POINT ( 'NONE',  ( 232.5999999999999659, -32.81249999999999289, 97.00000000000000000 ) ) ;
#765 = DIRECTION ( 'NONE',  ( 0.000000000000000000, -0.000000000000000000, 1.000000000000000000 ) ) ;
#766 = CARTESIAN_POINT ( 'NONE',  ( 85.15643035624999868, -31.11562499938548854, 98.40857419181659793 ) ) ;
#767 = FACE_OUTER_BOUND ( 'NONE', #5223, .T. ) ;
#768 = CARTESIAN_POINT ( 'NONE',  ( 81.02178482187500208, -30.55312499938548854, -102.3871387122750889 ) ) ;
#769 = DIRECTION ( 'NONE',  ( 1.000000000000000000, -1.387778780781445676E-15, -2.407412430484046130E-31 ) ) ;
#770 = EDGE_CURVE ( 'NONE', #14464, #4492, #1482, .T. ) ;
#771 = EDGE_LOOP ( 'NONE', ( #14055, #7466, #18393 ) ) ;
#772 = CARTESIAN_POINT ( 'NONE',  ( 79.39999999999999147, -30.65624999877096712, 98.26794919243113213 ) ) ;
#773 = APPLICATION_PROTOCOL_DEFINITION ( 'draft international standard', 'automotive_design', 1998, #7950 ) ;
#774 = CARTESIAN_POINT ( 'NONE',  ( 235.3564303562499447, -32.27812499938548285, 99.99999999999998579 ) ) ;
#775 = CARTESIAN_POINT ( 'NONE',  ( 232.5999999999999375, -32.16562499938547859, -53.18285161636690361 ) ) ;
#776 = CARTESIAN_POINT ( 'NONE',  ( -79.64356964374999848, -33.51562499938548711, 99.99999999999998579 ) ) ;
#777 = CYLINDRICAL_SURFACE ( 'NONE', #18363, 3.000000000000002665 ) ;
#778 = ORIENTED_EDGE ( 'NONE', *, *, #4094, .F. ) ;
#779 = VERTEX_POINT ( 'NONE', #3045 ) ;
#780 = CARTESIAN_POINT ( 'NONE',  ( -83.77821517812500929, -32.31562499938548427, -97.61286128772489690 ) ) ;
#781 = CARTESIAN_POINT ( 'NONE',  ( -82.39999999999999147, -33.65624999877097423, -103.0000000000000000 ) ) ;
#782 = EDGE_CURVE ( 'NONE', #14464, #6163, #17546, .T. ) ;
#783 = EDGE_LOOP ( 'NONE', ( #3113, #7017, #8709, #2513 ) ) ;
#784 = CARTESIAN_POINT ( 'NONE',  ( 82.39999999999999147, -32.84062499938548996, 96.81714838363319586 ) ) ;
#785 = CARTESIAN_POINT ( 'NONE',  ( -85.40000000000000568, -34.40624999877096712, -98.26794919243111792 ) ) ;
#786 = CARTESIAN_POINT ( 'NONE',  ( 84.69814068649969840, -35.00052333152936512, 101.9283540611242955 ) ) ;
#787 = DIRECTION ( 'NONE',  ( -1.000000000000000000, 1.387778780781445478E-15, 2.407412430484046130E-31 ) ) ;
#788 = CARTESIAN_POINT ( 'NONE',  ( -85.40000000000000568, -31.70624999877096784, 101.7320508075688679 ) ) ;
#789 = CARTESIAN_POINT ( 'NONE',  ( -85.40000000000000568, -33.09374999877096712, 99.99999999999998579 ) ) ;
#790 = CARTESIAN_POINT ( 'NONE',  ( 85.00132729415355470, -35.00000000000000711, -101.2112556744910563 ) ) ;
#791 = PRODUCT ( 'tray', 'tray', '', ( #18646 ) ) ;
#792 = DIRECTION ( 'NONE',  ( 0.000000000000000000, 0.000000000000000000, 1.000000000000000000 ) ) ;
#793 = CARTESIAN_POINT ( 'NONE',  ( 234.1936318287815197, -32.00000000000000711, 102.4696265554870678 ) ) ;
#794 = CARTESIAN_POINT ( 'NONE',  ( 232.5999999999999375, -32.95312499938548001, 96.81714838363319586 ) ) ;
#795 = EDGE_LOOP ( 'NONE', ( #1159, #6294, #4402, #9977 ) ) ;
#796 = CARTESIAN_POINT ( 'NONE',  ( 85.15643035625001289, -32.42812499938548854, -98.40857419181659793 ) ) ;
#797 = CARTESIAN_POINT ( 'NONE',  ( 234.0999999999999375, -30.54374999877096286, 97.40192378864668399 ) ) ;
#798 = CARTESIAN_POINT ( 'NONE',  ( 235.5999999999999943, -31.10624999877096286, -48.26794919243124582 ) ) ;
#799 =( BOUNDED_CURVE ( )  B_SPLINE_CURVE ( 2, ( #10926, #13757, #590, #3595, #684, #1937, #18265, #395, #18168 ),
 .UNSPECIFIED., .F., .F. ) 
 B_SPLINE_CURVE_WITH_KNOTS ( ( 3, 2, 2, 2, 3 ),
 ( 0.5208333333333333703, 0.5277777777777777901, 0.5416666666666666297, 0.5555555555555555802, 0.5625000000000000000 ),
 .UNSPECIFIED. ) 
 CURVE ( )  GEOMETRIC_REPRESENTATION_ITEM ( )  RATIONAL_B_SPLINE_CURVE ( ( 0.9330127018922192983, 0.9330127018922198534, 1.000000000000000000, 0.8660254037844387076, 1.000000000000000000, 0.8660254037844387076, 1.000000000000000000, 0.9330127018922194093, 0.9330127018922194093 ) ) 
 REPRESENTATION_ITEM ( '' )  );
#800 = VERTEX_POINT ( 'NONE', #18004 ) ;
#801 = CARTESIAN_POINT ( 'NONE',  ( 231.7961524227065695, -34.59240381056765301, 96.99999999999997158 ) ) ;
#802 = CARTESIAN_POINT ( 'NONE',  ( 0.1217565302851051218, -2.351289329882176204, -2.927447417349502423 ) ) ;
#803 = CARTESIAN_POINT ( 'NONE',  ( -4.211140560182196957, 2.431303136016537803, -3.745885042887433514 ) ) ;
#804 = VERTEX_POINT ( 'NONE', #7538 ) ;
#805 = CARTESIAN_POINT ( 'NONE',  ( -85.15643035625001289, -30.25312499938548783, 99.99999999999998579 ) ) ;
#806=STYLED_ITEM('',(#19357),#9467);
#807 = LINE ( 'NONE', #9075, #14712 ) ;
#808 = ORIENTED_EDGE ( 'NONE', *, *, #18816, .F. ) ;
#809 =( LENGTH_UNIT ( ) NAMED_UNIT ( * ) SI_UNIT ( .MILLI., .METRE. ) );
#810 = CARTESIAN_POINT ( 'NONE',  ( 80.90000000000000568, -33.45000000000000284, -102.5980762113533018 ) ) ;
#811 = CARTESIAN_POINT ( 'NONE',  ( -83.20384757729337366, -30.48615380933863150, 97.00000000000000000 ) ) ;
#812 = CARTESIAN_POINT ( 'NONE',  ( -80.90000000000000568, -35.19374999877096855, 102.5980762113533018 ) ) ;
#813 = CARTESIAN_POINT ( 'NONE',  ( -79.39999999999999147, -30.63750000000000284, 98.26794919243110371 ) ) ;
#814 = ADVANCED_FACE ( 'NONE', ( #136 ), #4908, .F. ) ;
#815 = CARTESIAN_POINT ( 'NONE',  ( 233.5140320577117166, -35.00000000000000711, -52.81360193307793338 ) ) ;
#816 = CYLINDRICAL_SURFACE ( 'NONE', #7870, 3.000000000000009770 ) ;
#817 = CARTESIAN_POINT ( 'NONE',  ( 79.64356964374998427, -34.49062499938548854, -98.40857419181659793 ) ) ;
#818 = DIRECTION ( 'NONE',  ( 0.000000000000000000, 0.000000000000000000, 1.000000000000000000 ) ) ;
#819 = CARTESIAN_POINT ( 'NONE',  ( -79.64356964375001269, -32.20312499938548001, 101.5914258081833879 ) ) ;
#820 = AXIS2_PLACEMENT_3D ( 'NONE', #14217, #14502, #3869 ) ;
#821 = DIRECTION ( 'NONE',  ( 1.000000000000000000, 0.000000000000000000, -0.000000000000000000 ) ) ;
#822 = ORIENTED_EDGE ( 'NONE', *, *, #3264, .T. ) ;
#823 = CARTESIAN_POINT ( 'NONE',  ( 235.5999999999999943, -34.23749999999999716, -51.73205080756900287 ) ) ;
#824 = CARTESIAN_POINT ( 'NONE',  ( 233.4038475772932770, -33.22634618820329422, -53.00000000000011369 ) ) ;
#825 = B_SPLINE_CURVE_WITH_KNOTS ( 'NONE', 3,
 ( #10025, #11490, #16078, #19109, #7092, #14796, #5637, #14603, #19208, #11583, #2686, #5729, #17454, #4257, #5823, #8742, #8643, #2588 ),
 .UNSPECIFIED., .F., .F.,
 ( 4, 2, 2, 2, 2, 2, 2, 2, 4 ),
 ( 0.000000000000000000, 0.0007106627595359116300, 0.001421325519071823260, 0.002131988278607734998, 0.002842651038143646520, 0.003553313797679558041, 0.004263976557215469997, 0.004974639316751381518, 0.005685302076287293040 ),
 .UNSPECIFIED. ) ;
#826 = FACE_OUTER_BOUND ( 'NONE', #7143, .T. ) ;
#827 = CARTESIAN_POINT ( 'NONE',  ( 85.40000000000000568, -33.60000000000000142, 99.99999999999998579 ) ) ;
#828 = CARTESIAN_POINT ( 'NONE',  ( -79.64356964375001269, -34.49062499938548854, 98.40857419181659793 ) ) ;
#829 = CARTESIAN_POINT ( 'NONE',  ( 231.2217848218749339, -30.21562499938547575, -52.38713871227520968 ) ) ;
#830 = ORIENTED_EDGE ( 'NONE', *, *, #9352, .T. ) ;
#831 = ADVANCED_FACE ( 'NONE', ( #1967 ), #1871, .F. ) ;
#832 = CARTESIAN_POINT ( 'NONE',  ( 249.9999999999999716, -29.80000000000000426, 150.0000000000000000 ) ) ;
#833 = CIRCLE ( 'NONE', #11436, 6.000000000000015987 ) ;
#834 = CARTESIAN_POINT ( 'NONE',  ( 234.0999999999999375, -33.89999999999999147, -47.40192378864679768 ) ) ;
#835 = CARTESIAN_POINT ( 'NONE',  ( 85.15643035625001289, -31.94062499938548427, 99.99999999999998579 ) ) ;
#836 = CARTESIAN_POINT ( 'NONE',  ( 113.0000000000000000, 10.39615242270649276, -145.9967928284264076 ) ) ;
#837 = CARTESIAN_POINT ( 'NONE',  ( -82.39999999999999147, -33.51562499938548711, 96.81714838363319586 ) ) ;
#838 = CARTESIAN_POINT ( 'NONE',  ( 84.44763168836732348, -32.00000000000002132, 98.15470523285560489 ) ) ;
#839 = CARTESIAN_POINT ( 'NONE',  ( 85.15643035625001289, -32.84062499938548285, 99.99999999999998579 ) ) ;
#840 = CARTESIAN_POINT ( 'NONE',  ( 79.64356964375001269, -33.21562499938548996, -101.5914258081833879 ) ) ;
#841 = CARTESIAN_POINT ( 'NONE',  ( 235.3564303562499447, -33.06562499938547717, -50.00000000000011369 ) ) ;
#842 = CARTESIAN_POINT ( 'NONE',  ( -79.64356964374998427, -34.45312499938548711, 101.5914258081833879 ) ) ;
#843 = ORIENTED_EDGE ( 'NONE', *, *, #17616, .T. ) ;
#844 = CARTESIAN_POINT ( 'NONE',  ( 85.15643035624999868, -32.09062499938548996, 101.5914258081833879 ) ) ;
#845 = CARTESIAN_POINT ( 'NONE',  ( 4.141042297810615835, -2.227970268150433863, -3.687027686973623819 ) ) ;
#846 = CARTESIAN_POINT ( 'NONE',  ( -80.90000000000000568, -34.35000000000000853, 102.5980762113533018 ) ) ;
#847 = CARTESIAN_POINT ( 'NONE',  ( -82.39999999999999147, -30.92812499938548143, 103.1828516163667899 ) ) ;
#848 = CARTESIAN_POINT ( 'NONE',  ( -85.15643035625001289, -31.94062499938548427, 99.99999999999998579 ) ) ;
#849 = PLANE ( 'NONE',  #7119 ) ;
#850 = ORIENTED_EDGE ( 'NONE', *, *, #11503, .F. ) ;
#851 = CARTESIAN_POINT ( 'NONE',  ( -79.39999999999999147, -34.23750000000000426, -101.7320508075688821 ) ) ;
#852 = DIRECTION ( 'NONE',  ( 0.000000000000000000, 0.000000000000000000, 1.000000000000000000 ) ) ;
#853 = CYLINDRICAL_SURFACE ( 'NONE', #4855, 3.000000000000002665 ) ;
#854 = CARTESIAN_POINT ( 'NONE',  ( -85.40000000000000568, -30.48356250001229029, 98.26794919243111792 ) ) ;
#855 = CIRCLE ( 'NONE', #7750, 2.649999999999982148 ) ;
#856 = B_SPLINE_CURVE_WITH_KNOTS ( 'NONE', 3,
 ( #6018, #19210, #16276, #18130, #2978, #19312 ),
 .UNSPECIFIED., .F., .F.,
 ( 4, 2, 4 ),
 ( 0.002044882221487522803, 0.003063384235218489376, 0.004081886248949456383 ),
 .UNSPECIFIED. ) ;
#857 = CARTESIAN_POINT ( 'NONE',  ( -85.40000000000000568, -34.53750000000000142, 98.26794919243111792 ) ) ;
#858 = CARTESIAN_POINT ( 'NONE',  ( -80.90000000000000568, -32.94374999877096855, 102.5980762113533018 ) ) ;
#859 = CYLINDRICAL_SURFACE ( 'NONE', #3213, 3.000000000000002665 ) ;
#860 = CARTESIAN_POINT ( 'NONE',  ( 79.64356964374998427, -34.82812499938548711, 101.5914258081833879 ) ) ;
#861 = CARTESIAN_POINT ( 'NONE',  ( 85.15643035624999868, -30.74062499938548143, 101.5914258081833879 ) ) ;
#862 = CARTESIAN_POINT ( 'NONE',  ( 232.1470656674051440, -31.99999999999999289, 97.19890519204298585 ) ) ;
#863 = VECTOR ( 'NONE', #18702, 1000.000000000000000 ) ;
#864 = CARTESIAN_POINT ( 'NONE',  ( -85.40000000000000568, -32.73750000000000426, -101.7320508075688821 ) ) ;
#865 = CARTESIAN_POINT ( 'NONE',  ( 83.77821517812500929, -31.22812499938548569, -97.61286128772489690 ) ) ;
#866 = CARTESIAN_POINT ( 'NONE',  ( 81.59615242270662350, -32.96115380933864003, 97.00000000000000000 ) ) ;
#867 = VERTEX_POINT ( 'NONE', #16826 ) ;
#868 = DIRECTION ( 'NONE',  ( -1.000000000000000000, 1.387778780781445676E-15, 2.407412430484046130E-31 ) ) ;
#869 = CARTESIAN_POINT ( 'NONE',  ( 234.8201511961207757, -35.00000000000002132, -48.35655086105373357 ) ) ;
#870 = CARTESIAN_POINT ( 'NONE',  ( 229.8435696437499871, -32.91562499938547859, -48.40857419181671162 ) ) ;
#871 = VECTOR ( 'NONE', #3828, 1000.000000000000000 ) ;
#872 = PRESENTATION_LAYER_ASSIGNMENT (  '', '', ( #17080 ) ) ;
#873 = CARTESIAN_POINT ( 'NONE',  ( -79.64356964375001269, -33.10312499938549280, 101.5914258081833879 ) ) ;
#874 = FACE_OUTER_BOUND ( 'NONE', #685, .T. ) ;
#875 = EDGE_LOOP ( 'NONE', ( #11455, #8700, #7987, #17282 ) ) ;
#876 = CARTESIAN_POINT ( 'NONE',  ( -82.39999999999999147, -31.15312499938548640, -103.1828516163667899 ) ) ;
#877 = FACE_OUTER_BOUND ( 'NONE', #6470, .T. ) ;
#878 = ORIENTED_EDGE ( 'NONE', *, *, #756, .T. ) ;
#879 = CARTESIAN_POINT ( 'NONE',  ( 83.77821517812500929, -34.37812499938548427, 102.3871387122750889 ) ) ;
#880 = VECTOR ( 'NONE', #2468, 1000.000000000000000 ) ;
#881 = CARTESIAN_POINT ( 'NONE',  ( -85.40000000000000568, -35.34374999877096712, -99.99999999999998579 ) ) ;
#882 = CARTESIAN_POINT ( 'NONE',  ( 85.40000000000000568, -34.91250000000000142, 98.26794919243111792 ) ) ;
#883 = CARTESIAN_POINT ( 'NONE',  ( 79.39999999999999147, -34.63124999877096855, -98.26794919243110371 ) ) ;
#884 = CARTESIAN_POINT ( 'NONE',  ( -82.39999999999999147, -31.63124999877097210, 103.4641016151377499 ) ) ;
#885 = CARTESIAN_POINT ( 'NONE',  ( -85.40000000000000568, -35.36739044046696279, 98.90809476984486537 ) ) ;
#886 = VECTOR ( 'NONE', #2876, 1000.000000000000000 ) ;
#887 = CARTESIAN_POINT ( 'NONE',  ( -79.64356964374998427, -32.57812499938548711, -101.5914258081833879 ) ) ;
#888 = VECTOR ( 'NONE', #17237, 1000.000000000000000 ) ;
#889 = CARTESIAN_POINT ( 'NONE',  ( -82.40000000000000568, -34.10624999877096997, -102.9999999999999858 ) ) ;
#890 = LINE ( 'NONE', #18471, #3199 ) ;
#891 = CARTESIAN_POINT ( 'NONE',  ( 231.0999999999999375, -30.37499999999999645, 102.5980762113533018 ) ) ;
#892 = EDGE_CURVE ( 'NONE', #2299, #18536, #6552, .T. ) ;
#893 = VERTEX_POINT ( 'NONE', #7634 ) ;
#894 = AXIS2_PLACEMENT_3D ( 'NONE', #15497, #16581, #278 ) ;
#895 = CARTESIAN_POINT ( 'NONE',  ( -81.02178482187500208, -34.94062499938548427, -97.61286128772489690 ) ) ;
#896 = CARTESIAN_POINT ( 'NONE',  ( 234.0999999999999375, -32.04374999877096286, -47.40192378864679768 ) ) ;
#897 = ORIENTED_EDGE ( 'NONE', *, *, #8064, .F. ) ;
#898 = CARTESIAN_POINT ( 'NONE',  ( 229.5999999999999375, -32.64374999877096428, 99.99999999999998579 ) ) ;
#899 = CARTESIAN_POINT ( 'NONE',  ( -82.39999999999999147, -30.47812499938548569, 103.1828516163667899 ) ) ;
#900 = CARTESIAN_POINT ( 'NONE',  ( -0.3461262719736137305, 4.658553426539289610, -3.671615880910373608 ) ) ;
#901 = ORIENTED_EDGE ( 'NONE', *, *, #18919, .F. ) ;
#902 = CARTESIAN_POINT ( 'NONE',  ( 232.5999999999999091, -33.03749999999998721, -47.00000000000011369 ) ) ;
#903 = CARTESIAN_POINT ( 'NONE',  ( 99.99999999999994316, -35.00000000000000000, -150.0000000000000000 ) ) ;
#904 = ORIENTED_EDGE ( 'NONE', *, *, #13663, .T. ) ;
#905 = ADVANCED_FACE ( 'NONE', ( #18104, #4715 ), #15646, .F. ) ;
#906 = CARTESIAN_POINT ( 'NONE',  ( 85.40000000000000568, -32.66250000000000142, -101.7320508075688679 ) ) ;
#907 = DIRECTION ( 'NONE',  ( -0.000000000000000000, -0.000000000000000000, 1.000000000000000000 ) ) ;
#908 = EDGE_CURVE ( 'NONE', #13473, #10972, #10673, .T. ) ;
#909 = CARTESIAN_POINT ( 'NONE',  ( -79.64356964375001269, -30.89062499938548711, 98.40857419181659793 ) ) ;
#910 = CARTESIAN_POINT ( 'NONE',  ( -83.90000000000000568, -33.97106250001230165, 102.5980762113533018 ) ) ;
#911 = CARTESIAN_POINT ( 'NONE',  ( 4.203833317240879275, 1.627343821129582979, -3.597273115243889929 ) ) ;
#912 = CARTESIAN_POINT ( 'NONE',  ( 233.0909187468006678, -31.99999999999998579, -52.83814945501250548 ) ) ;
#913 = EDGE_CURVE ( 'NONE', #11406, #10162, #13170, .T. ) ;
#914 = CARTESIAN_POINT ( 'NONE',  ( 82.39999999999999147, -34.86562499938548854, -96.81714838363319586 ) ) ;
#915 = CYLINDRICAL_SURFACE ( 'NONE', #17436, 3.000000000000002665 ) ;
#916 = CARTESIAN_POINT ( 'NONE',  ( -81.02178482187500208, -32.24062499938548854, 102.3871387122750889 ) ) ;
#917 =( BOUNDED_CURVE ( )  B_SPLINE_CURVE ( 2, ( #8964, #4479, #7598, #11995, #3006, #16396, #4288, #14932, #1556 ),
 .UNSPECIFIED., .F., .F. ) 
 B_SPLINE_CURVE_WITH_KNOTS ( ( 3, 2, 2, 2, 3 ),
 ( 0.2708333333333333148, 0.2777777777777777901, 0.2916666666666666852, 0.3055555555555555802, 0.3125000000000001110 ),
 .UNSPECIFIED. ) 
 CURVE ( )  GEOMETRIC_REPRESENTATION_ITEM ( )  RATIONAL_B_SPLINE_CURVE ( ( 0.9330127018922194093, 0.9330127018922190762, 1.000000000000000000, 0.8660254037844387076, 1.000000000000000000, 0.8660254037844387076, 1.000000000000000000, 0.9330127018922182991, 0.9330127018922194093 ) ) 
 REPRESENTATION_ITEM ( '' )  );
#918 = DIRECTION ( 'NONE',  ( 1.000000000000000000, -0.000000000000000000, -2.407412430484046130E-31 ) ) ;
#919 = ORIENTED_EDGE ( 'NONE', *, *, #16886, .F. ) ;
#920 = CARTESIAN_POINT ( 'NONE',  ( 230.3018593135002448, -35.00052333152935802, -51.92835406112443053 ) ) ;
#921 = CARTESIAN_POINT ( 'NONE',  ( -82.40000000000000568, -30.00000000000000355, -99.99999999999998579 ) ) ;
#922 = LINE ( 'NONE', #17517, #863 ) ;
#923 = CARTESIAN_POINT ( 'NONE',  ( 232.5999999999999943, -33.96562499938547575, 96.81714838363319586 ) ) ;
#924 = CARTESIAN_POINT ( 'NONE',  ( -79.64356964375001269, -35.01562499938548711, 101.5914258081833879 ) ) ;
#925 = EDGE_CURVE ( 'NONE', #14097, #6590, #7774, .T. ) ;
#926 = CARTESIAN_POINT ( 'NONE',  ( 229.8435696437499871, -30.62812499938547717, -51.59142580818350865 ) ) ;
#927 = VERTEX_POINT ( 'NONE', #3719 ) ;
#928 = CARTESIAN_POINT ( 'NONE',  ( -82.30067660862302148, -35.00052948526250418, 96.98128288508057437 ) ) ;
#929 = CARTESIAN_POINT ( 'NONE',  ( -85.15643035624999868, -34.67812499938548143, 98.40857419181659793 ) ) ;
#930 = CARTESIAN_POINT ( 'NONE',  ( -82.40000000000000568, -35.00000000000000000, 107.5000000000000142 ) ) ;
#931 = CARTESIAN_POINT ( 'NONE',  ( 83.77821517812500929, -31.86562499938548498, 97.61286128772489690 ) ) ;
#932 = LINE ( 'NONE', #5430, #6200 ) ;
#933 = CARTESIAN_POINT ( 'NONE',  ( 232.5999999999999943, -32.50312499938547717, -53.18285161636690361 ) ) ;
#934 = ADVANCED_FACE ( 'NONE', ( #12608 ), #616, .T. ) ;
#935 = CARTESIAN_POINT ( 'NONE',  ( -79.64356964374998427, -34.56562499938548427, 101.5914258081833879 ) ) ;
#936 = CARTESIAN_POINT ( 'NONE',  ( -83.77821517812500929, -33.92812499938548854, -102.3871387122750889 ) ) ;
#937 = CARTESIAN_POINT ( 'NONE',  ( 79.64356964375001269, -32.65312499938548285, 98.40857419181659793 ) ) ;
#938 = CARTESIAN_POINT ( 'NONE',  ( 79.64356964375001269, -34.11562499938548854, -101.5914258081833879 ) ) ;
#939 = CARTESIAN_POINT ( 'NONE',  ( 233.9782151781249411, -34.04062499938547859, -47.61286128772501769 ) ) ;
#940 = CARTESIAN_POINT ( 'NONE',  ( -79.64356964374998427, -33.55312499938548854, 101.5914258081833879 ) ) ;
#941 = CARTESIAN_POINT ( 'NONE',  ( 79.64356964374999848, -30.81562499938548427, -99.99999999999998579 ) ) ;
#942 = ORIENTED_EDGE ( 'NONE', *, *, #12020, .F. ) ;
#943 = DIRECTION ( 'NONE',  ( 1.000000000000000000, -1.387778780781445676E-15, -2.407412430484046130E-31 ) ) ;
#944 = CARTESIAN_POINT ( 'NONE',  ( 231.0999999999999375, -32.32499999999999574, 97.40192378864668399 ) ) ;
#945 = EDGE_CURVE ( 'NONE', #2644, #11697, #6762, .T. ) ;
#946 = CARTESIAN_POINT ( 'NONE',  ( -80.90000000000000568, -33.45000000000000284, 102.5980762113533018 ) ) ;
#947 = UNCERTAINTY_MEASURE_WITH_UNIT (LENGTH_MEASURE( 1.000000000000000082E-05 ), #8507, 'distance_accuracy_value', 'NONE');
#948 = CARTESIAN_POINT ( 'NONE',  ( -85.15643035624999868, -31.00312499938548072, 101.5914258081833879 ) ) ;
#949 = CARTESIAN_POINT ( 'NONE',  ( -79.64356964374999848, -30.81562499938548427, 99.99999999999998579 ) ) ;
#950 = CARTESIAN_POINT ( 'NONE',  ( -83.90000000000000568, -31.42500000000000071, 97.40192378864668399 ) ) ;
#951 = ORIENTED_EDGE ( 'NONE', *, *, #14019, .F. ) ;
#952 = CARTESIAN_POINT ( 'NONE',  ( -82.39999999999999147, -33.26250000000000284, -103.4641016151377499 ) ) ;
#953 = PRODUCT_DEFINITION_SHAPE ( 'NONE', 'NONE',  #19328 ) ;
#954 = CARTESIAN_POINT ( 'NONE',  ( -82.40000000000000568, -30.00000000000000355, 99.99999999999998579 ) ) ;
#955 = CARTESIAN_POINT ( 'NONE',  ( -99.99999999999998579, 0.000000000000000000, -150.0000000000000000 ) ) ;
#956 = CARTESIAN_POINT ( 'NONE',  ( -85.40000000000000568, -30.93356250001229313, 98.26794919243111792 ) ) ;
#957 = CYLINDRICAL_SURFACE ( 'NONE', #2043, 3.000000000000002665 ) ;
#958 = CARTESIAN_POINT ( 'NONE',  ( 1.567478505476134803E-15, 4.618802153517012954, -3.504269196027872457 ) ) ;
#959 = CARTESIAN_POINT ( 'NONE',  ( -85.15643035625001289, -30.59062499938548285, 99.99999999999998579 ) ) ;
#960 = DIRECTION ( 'NONE',  ( 0.000000000000000000, 0.000000000000000000, -1.000000000000000000 ) ) ;
#961 = CARTESIAN_POINT ( 'NONE',  ( -85.40000000000000568, -33.09374999877096712, -99.99999999999998579 ) ) ;
#962 = CARTESIAN_POINT ( 'NONE',  ( -84.28136653320154892, -32.00000000000001421, 97.98546077809197641 ) ) ;
#963 = CARTESIAN_POINT ( 'NONE',  ( -82.40000000000001990, -32.53124999877097423, -97.00000000000000000 ) ) ;
#964 = CARTESIAN_POINT ( 'NONE',  ( 79.64356964375001269, -33.21562499938548996, -101.5914258081833879 ) ) ;
#965 = CARTESIAN_POINT ( 'NONE',  ( 5.384454397937118664, 0.000000000000000000, -4.484454397937119197 ) ) ;
#966 = ORIENTED_EDGE ( 'NONE', *, *, #1251, .T. ) ;
#967 = CARTESIAN_POINT ( 'NONE',  ( 80.90000000000000568, -31.44374999877096855, 102.5980762113533018 ) ) ;
#968 = CARTESIAN_POINT ( 'NONE',  ( 229.8435696437499871, -34.34062499938547575, 98.40857419181659793 ) ) ;
#969 = CARTESIAN_POINT ( 'NONE',  ( 233.9782151781249411, -33.70312499938548001, -47.61286128772501769 ) ) ;
#970 = CYLINDRICAL_SURFACE ( 'NONE', #13030, 2.649999999999985700 ) ;
#971 = CARTESIAN_POINT ( 'NONE',  ( -85.24876232368482931, -35.00000000000000711, -99.45334139305025190 ) ) ;
#972 = ORIENTED_EDGE ( 'NONE', *, *, #12588, .F. ) ;
#973 = CARTESIAN_POINT ( 'NONE',  ( -79.64356964375001269, -31.75312499938548427, -98.40857419181659793 ) ) ;
#974 = CARTESIAN_POINT ( 'NONE',  ( 80.90000000000000568, -32.34374999877096712, 102.5980762113533018 ) ) ;
#975 = EDGE_LOOP ( 'NONE', ( #10803, #15981, #15454, #9666, #3524 ) ) ;
#976 = CARTESIAN_POINT ( 'NONE',  ( 85.15643035625001289, -33.40312499938548285, 99.99999999999998579 ) ) ;
#977 = CARTESIAN_POINT ( 'NONE',  ( -85.15643035624999868, -30.29062499938548925, -101.5914258081833879 ) ) ;
#978 = CARTESIAN_POINT ( 'NONE',  ( -82.39999999999999147, -30.50624999877097210, -103.4641016151377499 ) ) ;
#979 = CARTESIAN_POINT ( 'NONE',  ( 231.2217848218749339, -30.32812499938548001, 97.61286128772489690 ) ) ;
#980 = CARTESIAN_POINT ( 'NONE',  ( -80.90000000000000568, -34.74374999877097281, 102.5980762113533018 ) ) ;
#981 = CARTESIAN_POINT ( 'NONE',  ( -85.15643035624999868, -31.56562499938548427, 101.5914258081833879 ) ) ;
#982 = CARTESIAN_POINT ( 'NONE',  ( -81.02178482187500208, -32.99062499938548854, -102.3871387122750889 ) ) ;
#983 = CARTESIAN_POINT ( 'NONE',  ( 233.7151113960924818, -35.00000000000000711, 102.5271494742949017 ) ) ;
#984 = CARTESIAN_POINT ( 'NONE',  ( 79.39999999999999147, -31.55624999877096926, -101.7320508075688537 ) ) ;
#985 = CARTESIAN_POINT ( 'NONE',  ( 231.0999999999999375, -31.27499999999999858, 102.5980762113533018 ) ) ;
#986 = EDGE_LOOP ( 'NONE', ( #10879, #13324, #8010, #1433 ) ) ;
#987 = CARTESIAN_POINT ( 'NONE',  ( 79.64356964374998427, -33.92812499938548854, -98.40857419181659793 ) ) ;
#988 = CARTESIAN_POINT ( 'NONE',  ( 234.0999999999999375, -33.69374999877096144, 97.40192378864668399 ) ) ;
#989 = CARTESIAN_POINT ( 'NONE',  ( 232.5999999999999375, -32.08124999877095718, -46.53589838486234953 ) ) ;
#990 = ORIENTED_EDGE ( 'NONE', *, *, #12505, .T. ) ;
#991 = CARTESIAN_POINT ( 'NONE',  ( -83.90000000000000568, -35.26874999877097139, 102.5980762113533018 ) ) ;
#992 = CARTESIAN_POINT ( 'NONE',  ( -82.40000000000001990, -32.30624999877097281, -103.0000000000000000 ) ) ;
#993 = DIRECTION ( 'NONE',  ( 0.000000000000000000, 0.000000000000000000, 1.000000000000000000 ) ) ;
#994 = ORIENTED_EDGE ( 'NONE', *, *, #2088, .F. ) ;
#995 = CARTESIAN_POINT ( 'NONE',  ( 4.175813232069151226, -4.122719923832748101, -3.898053888241413974E-16 ) ) ;
#996 = CARTESIAN_POINT ( 'NONE',  ( 229.5999999999999375, -33.05624999877096570, 101.7320508075688821 ) ) ;
#997 = ORIENTED_EDGE ( 'NONE', *, *, #5541, .F. ) ;
#998 = PRESENTATION_STYLE_ASSIGNMENT (( #11247 ) ) ;
#999 = CARTESIAN_POINT ( 'NONE',  ( 83.90000000000000568, -33.97500000000000853, -102.5980762113533018 ) ) ;
#1000 = CARTESIAN_POINT ( 'NONE',  ( 81.45486068924890333, -31.99999999999999289, -102.7533691519569885 ) ) ;
#1001 = EDGE_CURVE ( 'NONE', #18944, #3020, #12898, .T. ) ;
#1002 = ADVANCED_FACE ( 'NONE', ( #18772 ), #8405, .F. ) ;
#1003 = CARTESIAN_POINT ( 'NONE',  ( -79.64356964375001269, -31.86562499938548143, 101.5914258081833879 ) ) ;
#1004 = CARTESIAN_POINT ( 'NONE',  ( -80.90000000000000568, -32.85000000000000142, 97.40192378864668399 ) ) ;
#1005 = CARTESIAN_POINT ( 'NONE',  ( -82.40000000000000568, -30.00000000000000355, -99.99999999999998579 ) ) ;
#1006 = LINE ( 'NONE', #5601, #3813 ) ;
#1007 = DIRECTION ( 'NONE',  ( 0.000000000000000000, 0.000000000000000000, 1.000000000000000000 ) ) ;
#1008 = CARTESIAN_POINT ( 'NONE',  ( 0.000000000000000000, 0.000000000000000000, -4.974599999999998801 ) ) ;
#1009 = CYLINDRICAL_SURFACE ( 'NONE', #18973, 3.000000000000002665 ) ;
#1010 = PLANE ( 'NONE',  #18028 ) ;
#1011 = EDGE_LOOP ( 'NONE', ( #18338, #12679, #3902, #3454 ) ) ;
#1012 = CARTESIAN_POINT ( 'NONE',  ( 235.5999999999999943, -34.76249999999999574, -48.26794919243124582 ) ) ;
#1013 = CARTESIAN_POINT ( 'NONE',  ( -82.40000000000000568, -30.00000000000000355, 96.99999999999998579 ) ) ;
#1014 = AXIS2_PLACEMENT_3D ( 'NONE', #15088, #13614, #257 ) ;
#1015 = VECTOR ( 'NONE', #7998, 1000.000000000000000 ) ;
#1016 = EDGE_CURVE ( 'NONE', #17889, #804, #14357, .T. ) ;
#1017 = CARTESIAN_POINT ( 'NONE',  ( 4.175813232069148562, -2.061359961916374495, -3.570380186727398097 ) ) ;
#1018 = CARTESIAN_POINT ( 'NONE',  ( 229.8435696437499587, -33.89062499938548001, 98.40857419181659793 ) ) ;
#1019 = CARTESIAN_POINT ( 'NONE',  ( -82.39999999999999147, -33.74062499938548854, 103.1828516163667899 ) ) ;
#1020 = EDGE_CURVE ( 'NONE', #14645, #2256, #5419, .T. ) ;
#1021 = CARTESIAN_POINT ( 'NONE',  ( 229.8435696437499871, -31.07812499938548001, -51.59142580818350865 ) ) ;
#1022 = VERTEX_POINT ( 'NONE', #9780 ) ;
#1023 = CARTESIAN_POINT ( 'NONE',  ( -83.77821517812500929, -34.26562499938548711, 97.61286128772489690 ) ) ;
#1024 = CARTESIAN_POINT ( 'NONE',  ( -80.90000000000000568, -30.54374999877096997, 97.40192378864668399 ) ) ;
#1025 = CARTESIAN_POINT ( 'NONE',  ( 82.39999999999999147, -34.52812499938548996, 96.81714838363319586 ) ) ;
#1026 = CARTESIAN_POINT ( 'NONE',  ( 244.7999999999999545, -35.00000000000000000, -100.0000000000000000 ) ) ;
#1027 = CARTESIAN_POINT ( 'NONE',  ( 231.2217848218749339, -32.31562499938547717, -47.61286128772501769 ) ) ;
#1028 = CARTESIAN_POINT ( 'NONE',  ( -83.77821517812500929, -33.02812499938548285, 97.61286128772489690 ) ) ;
#1029 = CARTESIAN_POINT ( 'NONE',  ( -79.64356964374998427, -34.56562499938548427, -98.40857419181659793 ) ) ;
#1030 = CARTESIAN_POINT ( 'NONE',  ( 83.77821517812500929, -31.86562499938548498, 97.61286128772489690 ) ) ;
#1031 = CARTESIAN_POINT ( 'NONE',  ( 79.64356964374999848, -34.97812499938548569, -99.99999999999998579 ) ) ;
#1032 = CARTESIAN_POINT ( 'NONE',  ( 235.3564303562499447, -32.16562499938547859, -50.00000000000011369 ) ) ;
#1033 = CARTESIAN_POINT ( 'NONE',  ( -79.64356964374998427, -34.00312499938548427, 101.5914258081833879 ) ) ;
#1034 = CARTESIAN_POINT ( 'NONE',  ( 82.39999999999999147, -30.92812499938548143, -103.1828516163667899 ) ) ;
#1035 = ORIENTED_EDGE ( 'NONE', *, *, #18905, .F. ) ;
#1036 = DIRECTION ( 'NONE',  ( 0.000000000000000000, -3.154042683594203897E-15, -1.000000000000000000 ) ) ;
#1037 = CARTESIAN_POINT ( 'NONE',  ( 3.951447005078449148, -1.347150628109125003, 3.500000000000000888 ) ) ;
#1038 = CARTESIAN_POINT ( 'NONE',  ( -83.90000000000000568, -33.22500000000000142, 97.40192378864668399 ) ) ;
#1039 = AXIS2_PLACEMENT_3D ( 'NONE', #9542, #18538, #13936 ) ;
#1040 = CARTESIAN_POINT ( 'NONE',  ( -79.64356964375001269, -33.55312499938548854, 101.5914258081833879 ) ) ;
#1041 = CARTESIAN_POINT ( 'NONE',  ( -85.15643035624999868, -30.62812499938548427, 98.40857419181659793 ) ) ;
#1042 = CARTESIAN_POINT ( 'NONE',  ( 232.5999999999999375, -34.16249999999999432, 96.99999999999998579 ) ) ;
#1043 = CLOSED_SHELL ( 'NONE', ( #15727, #1878, #15369, #14233, #4639, #15697, #12649, #17613, #16169, #5440, #19146 ) ) ;
#1044 = CARTESIAN_POINT ( 'NONE',  ( 233.9782151781249411, -32.69062499938547717, 102.3871387122750889 ) ) ;
#1045 = CARTESIAN_POINT ( 'NONE',  ( 113.0000000000000142, 15.19999999999997442, -150.0000000000000000 ) ) ;
#1046 = CARTESIAN_POINT ( 'NONE',  ( 82.39999999999999147, -33.48750000000000426, -103.0000000000000000 ) ) ;
#1047 = CARTESIAN_POINT ( 'NONE',  ( 0.6920835326022565237, 4.454600218803884459, -3.597382984111579862 ) ) ;
#1048 = EDGE_CURVE ( 'NONE', #18266, #6163, #11022, .T. ) ;
#1049 = CARTESIAN_POINT ( 'NONE',  ( -82.39999999999999147, -32.98124999877096286, 102.9999999999999858 ) ) ;
#1050 = CARTESIAN_POINT ( 'NONE',  ( -79.64356964375001269, -30.32812499938548711, 98.40857419181659793 ) ) ;
#1051 = CARTESIAN_POINT ( 'NONE',  ( 232.5999999999999375, -29.99999999999999645, -50.00000000000011369 ) ) ;
#1052 = CARTESIAN_POINT ( 'NONE',  ( -83.20384757729335945, -32.73615380933863150, -102.9999999999999716 ) ) ;
#1053 = CARTESIAN_POINT ( 'NONE',  ( 83.77821517812500929, -33.92812499938548854, -97.61286128772489690 ) ) ;
#1054 = CARTESIAN_POINT ( 'NONE',  ( 229.5999999999999375, -34.08749999999999147, 98.26794919243111792 ) ) ;
#1055 = ORIENTED_EDGE ( 'NONE', *, *, #18470, .T. ) ;
#1056 = CARTESIAN_POINT ( 'NONE',  ( 85.40000000000000568, -33.99374999877097281, 99.99999999999998579 ) ) ;
#1057 = CARTESIAN_POINT ( 'NONE',  ( 232.5999999999999375, -34.83749999999999147, 103.0000000000000000 ) ) ;
#1058 = CARTESIAN_POINT ( 'NONE',  ( 232.5999999999999375, -32.84062499938548285, -46.81714838363331666 ) ) ;
#1059 = CARTESIAN_POINT ( 'NONE',  ( -81.02178482187500208, -34.79062499938548569, 97.61286128772489690 ) ) ;
#1060 = CARTESIAN_POINT ( 'NONE',  ( 0.000000000000000000, 0.000000000000000000, 0.000000000000000000 ) ) ;
#1061 = ORIENTED_EDGE ( 'NONE', *, *, #15792, .T. ) ;
#1062 = CARTESIAN_POINT ( 'NONE',  ( -79.64356964375001269, -34.90312499938548285, -98.40857419181659793 ) ) ;
#1063 = DIRECTION ( 'NONE',  ( 0.000000000000000000, 0.000000000000000000, -1.000000000000000000 ) ) ;
#1064 = ORIENTED_EDGE ( 'NONE', *, *, #3609, .F. ) ;
#1065 = CARTESIAN_POINT ( 'NONE',  ( 79.64356964374998427, -32.69062499938548427, 101.5914258081833879 ) ) ;
#1066 = CARTESIAN_POINT ( 'NONE',  ( -79.64356964375001269, -30.96562499938548640, -98.40857419181659793 ) ) ;
#1067 = CARTESIAN_POINT ( 'NONE',  ( 79.39999999999999147, -34.31250000000000000, 98.26794919243113213 ) ) ;
#1068 = CARTESIAN_POINT ( 'NONE',  ( -94.79999999999999716, -32.00000000000000000, 150.0000000000000000 ) ) ;
#1069 = CARTESIAN_POINT ( 'NONE',  ( -82.39999999999999147, -35.23124999877096997, 103.4641016151377499 ) ) ;
#1070 = CARTESIAN_POINT ( 'NONE',  ( -85.40000000000000568, -35.34374999877096712, 99.99999999999998579 ) ) ;
#1071 = CARTESIAN_POINT ( 'NONE',  ( -82.39999999999999147, -32.95312499938548711, -103.1828516163667899 ) ) ;
#1072 = CARTESIAN_POINT ( 'NONE',  ( 235.1663847376153740, -35.00000000000000000, 101.0217260113606983 ) ) ;
#1073 = CARTESIAN_POINT ( 'NONE',  ( 83.90000000000000568, -30.91874999877096997, -97.40192378864668399 ) ) ;
#1074 = CARTESIAN_POINT ( 'NONE',  ( 231.0999999999999375, -30.52499999999999503, 97.40192378864668399 ) ) ;
#1075 = ORIENTED_EDGE ( 'NONE', *, *, #13319, .F. ) ;
#1076 = PLANE ( 'NONE',  #99 ) ;
#1077 = CARTESIAN_POINT ( 'NONE',  ( 229.5999999999999375, -31.74374999877096215, 99.99999999999998579 ) ) ;
#1078 = CARTESIAN_POINT ( 'NONE',  ( -82.40000000000000568, -30.00000000000000355, 103.0000000000000000 ) ) ;
#1079 = CARTESIAN_POINT ( 'NONE',  ( 231.0999999999999375, -34.42499999999999716, 102.5980762113533018 ) ) ;
#1080 = ADVANCED_FACE ( 'NONE', ( #6860 ), #15549, .T. ) ;
#1081 = CARTESIAN_POINT ( 'NONE',  ( -85.15643035625001289, -31.49062499938548498, 99.99999999999998579 ) ) ;
#1082 = ORIENTED_EDGE ( 'NONE', *, *, #1142, .F. ) ;
#1083 = EDGE_LOOP ( 'NONE', ( #7928, #14869 ) ) ;
#1084 = LINE ( 'NONE', #11915, #8796 ) ;
#1085 = ORIENTED_EDGE ( 'NONE', *, *, #3636, .F. ) ;
#1086 = CARTESIAN_POINT ( 'NONE',  ( 80.90000000000000568, -32.55000000000000426, -102.5980762113533018 ) ) ;
#1087 = CARTESIAN_POINT ( 'NONE',  ( 83.74167325096733805, -31.99999999999999289, -102.4658751321106536 ) ) ;
#1088 = CARTESIAN_POINT ( 'NONE',  ( -85.15643035625001289, -31.15312499938548996, 99.99999999999998579 ) ) ;
#1089 = CARTESIAN_POINT ( 'NONE',  ( -79.39999999999999147, -31.61250000000000071, 101.7320508075688537 ) ) ;
#1090 = DIRECTION ( 'NONE',  ( 0.3420201433256622736, 0.000000000000000000, -0.9396926207859106484 ) ) ;
#1091 = CARTESIAN_POINT ( 'NONE',  ( 83.77821517812500929, -34.37812499938548427, -97.61286128772489690 ) ) ;
#1092 = MANIFOLD_SOLID_BREP ( 'Boss-Extrude1', #16920 ) ;
#1093 = CARTESIAN_POINT ( 'NONE',  ( 3.961551342853838698, 2.319461885623308017, 2.982574167880918115 ) ) ;
#1094 = FACE_OUTER_BOUND ( 'NONE', #17811, .T. ) ;
#1095 = CARTESIAN_POINT ( 'NONE',  ( -79.39999999999999147, -31.08750000000000568, 98.26794919243110371 ) ) ;
#1096 = ORIENTED_EDGE ( 'NONE', *, *, #11672, .F. ) ;
#1097 = CARTESIAN_POINT ( 'NONE',  ( -81.02178482187500208, -30.44062499938548783, -97.61286128772489690 ) ) ;
#1098 = CARTESIAN_POINT ( 'NONE',  ( -82.40000000000000568, -30.00000000000000355, 103.0000000000000000 ) ) ;
#1099 =( GEOMETRIC_REPRESENTATION_CONTEXT ( 3 ) GLOBAL_UNCERTAINTY_ASSIGNED_CONTEXT ( ( #7539 ) ) GLOBAL_UNIT_ASSIGNED_CONTEXT ( ( #809, #14267, #11443 ) ) REPRESENTATION_CONTEXT ( 'NONE', 'WORKASPACE' ) );
#1100 = CARTESIAN_POINT ( 'NONE',  ( -3.455068668934486276, 2.624017327439035707, -3.316620875263955437 ) ) ;
#1101 = CARTESIAN_POINT ( 'NONE',  ( -85.40000000000000568, -34.91250000000000142, -98.26794919243111792 ) ) ;
#1102 = CARTESIAN_POINT ( 'NONE',  ( -79.64356964375001269, -34.04062499938549280, 98.40857419181659793 ) ) ;
#1103 = CARTESIAN_POINT ( 'NONE',  ( 110.0000000000000568, 5.199999999999976197, -150.0000000000000000 ) ) ;
#1104 = CARTESIAN_POINT ( 'NONE',  ( 235.3564303562499447, -34.97812499938547859, -50.00000000000011369 ) ) ;
#1105 = ORIENTED_EDGE ( 'NONE', *, *, #2418, .F. ) ;
#1106 = CARTESIAN_POINT ( 'NONE',  ( -82.39999999999999147, -33.85312499938547859, 96.81714838363319586 ) ) ;
#1107 = CARTESIAN_POINT ( 'NONE',  ( 85.40000000000000568, -32.19374999877096855, -99.99999999999998579 ) ) ;
#1108 = CARTESIAN_POINT ( 'NONE',  ( 81.02178482187500208, -34.04062499938548569, 97.61286128772489690 ) ) ;
#1109 = DIRECTION ( 'NONE',  ( 0.000000000000000000, 0.000000000000000000, -1.000000000000000000 ) ) ;
#1110 = CARTESIAN_POINT ( 'NONE',  ( 229.8435696437499871, -31.00312499938547361, 101.5914258081833879 ) ) ;
#1111 = AXIS2_PLACEMENT_3D ( 'NONE', #1706, #12161, #6016 ) ;
#1112 = EDGE_CURVE ( 'NONE', #11694, #3907, #10561, .T. ) ;
#1113 = CARTESIAN_POINT ( 'NONE',  ( 111.5987303322250597, 7.969082163015147380, -145.7054384624938166 ) ) ;
#1114 = CARTESIAN_POINT ( 'NONE',  ( -83.77821517812500929, -33.92812499938548854, 97.61286128772489690 ) ) ;
#1115 = CARTESIAN_POINT ( 'NONE',  ( -85.15643035625001289, -33.40312499938548285, -99.99999999999998579 ) ) ;
#1116 = CARTESIAN_POINT ( 'NONE',  ( 85.15643035624999868, -35.05312499938548143, 98.40857419181659793 ) ) ;
#1117 = CARTESIAN_POINT ( 'NONE',  ( 79.64356964374999848, -33.62812499938548427, -99.99999999999998579 ) ) ;
#1118 = CARTESIAN_POINT ( 'NONE',  ( 229.8435696437499303, -33.74062499938548143, -50.00000000000011369 ) ) ;
#1119 = CARTESIAN_POINT ( 'NONE',  ( -83.77821517812500929, -32.31562499938548427, 102.3871387122750889 ) ) ;
#1120 = CARTESIAN_POINT ( 'NONE',  ( 79.64356964374999848, -31.71562499938548285, -99.99999999999998579 ) ) ;
#1121 = EDGE_CURVE ( 'NONE', #4832, #16118, #561, .T. ) ;
#1122 = EDGE_LOOP ( 'NONE', ( #5152, #15546 ) ) ;
#1123 = CARTESIAN_POINT ( 'NONE',  ( 81.02178482187500208, -35.05312499938548854, 97.61286128772489690 ) ) ;
#1124 = CARTESIAN_POINT ( 'NONE',  ( 0.6640947660595348800, -4.471078309994175548, -3.602146406945708090 ) ) ;
#1125 = MANIFOLD_SOLID_BREP ( 'FlangeHexFillet', #15665 ) ;
#1126 = CARTESIAN_POINT ( 'NONE',  ( -80.90000000000000568, -34.20000000000000284, 97.40192378864668399 ) ) ;
#1127 = AXIS2_PLACEMENT_3D ( 'NONE', #14079, #907, #2259 ) ;
#1128 = CARTESIAN_POINT ( 'NONE',  ( -82.39999999999999147, -34.30312499938548143, 96.81714838363319586 ) ) ;
#1129 = CARTESIAN_POINT ( 'NONE',  ( -79.64356964374999848, -31.26562499938548356, 99.99999999999998579 ) ) ;
#1130 = ORIENTED_EDGE ( 'NONE', *, *, #13051, .F. ) ;
#1131 = CARTESIAN_POINT ( 'NONE',  ( -79.58826230849692251, -32.00000000000093792, -101.0460072438472139 ) ) ;
#1132 = CARTESIAN_POINT ( 'NONE',  ( 229.8435696437499303, -32.39062499938548001, 99.99999999999998579 ) ) ;
#1133 = CARTESIAN_POINT ( 'NONE',  ( 0.000000000000000000, 0.000000000000000000, -25.03750572909317285 ) ) ;
#1134 = CARTESIAN_POINT ( 'NONE',  ( -4.000000000000000000, -2.309401076758515803, -0.4999999999999995559 ) ) ;
#1135 = ADVANCED_FACE ( 'NONE', ( #13578 ), #13862, .F. ) ;
#1136 = EDGE_CURVE ( 'NONE', #1970, #5897, #16626, .T. ) ;
#1137 = CARTESIAN_POINT ( 'NONE',  ( 100.0000000000000000, 10.19999999999999396, -130.0000000000000000 ) ) ;
#1138 = CARTESIAN_POINT ( 'NONE',  ( -83.90000000000000568, -34.96874999877096712, 97.40192378864668399 ) ) ;
#1139 = DIRECTION ( 'NONE',  ( -0.5000000000000019984, -0.8660254037844375974, 0.000000000000000000 ) ) ;
#1140 = CARTESIAN_POINT ( 'NONE',  ( 84.85729912020866550, -31.99999999999998579, 98.73859666561313020 ) ) ;
#1141 = CARTESIAN_POINT ( 'NONE',  ( -82.39999999999999147, -33.20624999877097849, -102.9999999999999858 ) ) ;
#1142 = EDGE_CURVE ( 'NONE', #18598, #4852, #9158, .T. ) ;
#1143 = AXIS2_PLACEMENT_3D ( 'NONE', #8341, #9245, #14297 ) ;
#1144 = CARTESIAN_POINT ( 'NONE',  ( 82.40000000000000568, -30.00000000000000355, 103.0000000000000000 ) ) ;
#1145 = DIRECTION ( 'NONE',  ( -1.000000000000000000, 0.000000000000000000, 0.000000000000000000 ) ) ;
#1146 = CARTESIAN_POINT ( 'NONE',  ( 82.39999999999999147, -32.61562499938548854, -96.81714838363319586 ) ) ;
#1147 = DIRECTION ( 'NONE',  ( 0.000000000000000000, 0.000000000000000000, -1.000000000000000000 ) ) ;
#1148 = ORIENTED_EDGE ( 'NONE', *, *, #9637, .T. ) ;
#1149 = CARTESIAN_POINT ( 'NONE',  ( 80.90000000000000568, -33.39374999877097139, 97.40192378864668399 ) ) ;
#1150 = CARTESIAN_POINT ( 'NONE',  ( 231.2217848218749339, -33.92812499938548143, 97.61286128772489690 ) ) ;
#1151 = FACE_OUTER_BOUND ( 'NONE', #13156, .T. ) ;
#1152 = PRODUCT_DEFINITION_FORMATION_WITH_SPECIFIED_SOURCE ( 'ANY', '', #18891, .NOT_KNOWN. ) ;
#1153 = CARTESIAN_POINT ( 'NONE',  ( 235.5999999999999375, -34.21874999877096002, 99.99999999999998579 ) ) ;
#1154 = CARTESIAN_POINT ( 'NONE',  ( -84.06832524826180020, -35.00000000000001421, -97.74327260034003473 ) ) ;
#1155 = VERTEX_POINT ( 'NONE', #12694 ) ;
#1156 = EDGE_CURVE ( 'NONE', #7460, #2579, #7567, .T. ) ;
#1157 = CARTESIAN_POINT ( 'NONE',  ( -85.15643035624999868, -34.22812499938547859, -101.5914258081833879 ) ) ;
#1158 = AXIS2_PLACEMENT_3D ( 'NONE', #12215, #18183, #17530 ) ;
#1159 = ORIENTED_EDGE ( 'NONE', *, *, #47, .F. ) ;
#1160 = DIRECTION ( 'NONE',  ( -0.000000000000000000, -0.000000000000000000, 1.000000000000000000 ) ) ;
#1161 = CARTESIAN_POINT ( 'NONE',  ( -83.77821517812500929, -32.12812499938548427, -102.3871387122750889 ) ) ;
#1162 = CARTESIAN_POINT ( 'NONE',  ( -79.39999999999999147, -32.38124999877096855, -101.7320508075688821 ) ) ;
#1163 = DIRECTION ( 'NONE',  ( -0.000000000000000000, -0.000000000000000000, -1.000000000000000000 ) ) ;
#1164 = CARTESIAN_POINT ( 'NONE',  ( -83.90000000000000568, -33.61874999877097281, 97.40192378864668399 ) ) ;
#1165 = VECTOR ( 'NONE', #12606, 1000.000000000000000 ) ;
#1166 = CARTESIAN_POINT ( 'NONE',  ( -79.64356964374999848, -30.92812499938548498, 99.99999999999998579 ) ) ;
#1167 = DIRECTION ( 'NONE',  ( -0.000000000000000000, -1.000000000000000000, -0.000000000000000000 ) ) ;
#1168 = CARTESIAN_POINT ( 'NONE',  ( -81.59615242270662350, -34.12634618820329990, -102.9999999999999858 ) ) ;
#1169 = EDGE_CURVE ( 'NONE', #16799, #12847, #17295, .T. ) ;
#1170 = CARTESIAN_POINT ( 'NONE',  ( 82.39999999999999147, -30.95624999877097139, -96.53589838486223584 ) ) ;
#1171 = CIRCLE ( 'NONE', #2096, 2.199999999999993516 ) ;
#1172 = CARTESIAN_POINT ( 'NONE',  ( 229.5999999999999375, -31.79999999999999361, 99.99999999999998579 ) ) ;
#1173 = ORIENTED_EDGE ( 'NONE', *, *, #12327, .F. ) ;
#1174 = CARTESIAN_POINT ( 'NONE',  ( 233.4038475772933054, -34.76115380933863008, 102.9999999999999858 ) ) ;
#1175 =( NAMED_UNIT ( * ) PLANE_ANGLE_UNIT ( ) SI_UNIT ( $, .RADIAN. ) );
#1176 = CARTESIAN_POINT ( 'NONE',  ( 235.5999999999999943, -31.93124999877096570, 98.26794919243110371 ) ) ;
#1177 = CARTESIAN_POINT ( 'NONE',  ( 231.0999999999999375, -31.36874999877096215, -52.59807621135342970 ) ) ;
#1178 = CARTESIAN_POINT ( 'NONE',  ( 231.0999999999999375, -32.71874999877096002, 97.40192378864668399 ) ) ;
#1179 = CARTESIAN_POINT ( 'NONE',  ( -79.64356964374998427, -31.30312499938548143, 101.5914258081833879 ) ) ;
#1180 = VECTOR ( 'NONE', #3831, 1000.000000000000000 ) ;
#1181 = EDGE_LOOP ( 'NONE', ( #9170, #1259, #4978, #13735 ) ) ;
#1182 = ORIENTED_EDGE ( 'NONE', *, *, #338, .T. ) ;
#1183 = CARTESIAN_POINT ( 'NONE',  ( -4.197393957002303999, 0.4069871074557429025, -3.503767560748926257 ) ) ;
#1184 = CARTESIAN_POINT ( 'NONE',  ( 4.175075985190098926, -4.120741555260250877, -7.642383270497488377E-15 ) ) ;
#1185 = ORIENTED_EDGE ( 'NONE', *, *, #1121, .T. ) ;
#1186 =( BOUNDED_CURVE ( )  B_SPLINE_CURVE ( 2, ( #8849, #13347, #16478, #11785, #17757, #4364, #13625, #6222, #12169, #7485, #16376, #3082, #169, #10324, #18137, #4757, #16666, #10700, #13440, #6026, #14805, #19320, #2985, #5931, #74, #11878, #3373, #14017, #16860, #12645, #7961, #5043, #3465, #9524, #2291, #3664, #10984, #17149, #15687, #3565, #15391, #746, #16953, #11186, #5137, #2002, #11082, #17052, #9628, #18233, #6315, #18619, #10892, #8160, #13915, #15590, #9423, #8062, #12269, #6408, #1904, #16757, #14109, #653, #12363, #553, #2102, #6701, #5237, #4950, #12549, #6511, #15289, #18331, #3756, #15490, #12456, #9325, #6601, #18520, #9721, #7866, #18422 ),
 .UNSPECIFIED., .F., .F. ) 
 B_SPLINE_CURVE_WITH_KNOTS ( ( 3, 2, 2, 2, 2, 2, 2, 2, 2, 2, 2, 2, 2, 2, 2, 2, 2, 2, 2, 2, 2, 2, 2, 2, 2, 2, 2, 2, 2, 2, 2, 2, 2, 2, 2, 2, 2, 2, 2, 2, 2, 3 ),
 ( 0.3495698921800953207, 0.3600184345287980592, 0.3750192026341646057, 0.3900199707395312076, 0.4050207388448978096, 0.4200215069502644116, 0.4350222750556309581, 0.4500230431609975601, 0.4650238112663641621, 0.4800245793717307086, 0.4950253474770972550, 0.5100261155824639125, 0.5250268836878304590, 0.5400276517931970055, 0.5550284198985635520, 0.5700291880039302095, 0.5850299561092967560, 0.6000307242146634135, 0.6150314923200299599, 0.6300322604253965064, 0.6450330285307630529, 0.6600337966361298214, 0.6750345647414962569, 0.6900353328468628034, 0.7050361009522294609, 0.7200368690575960073, 0.7350376371629625538, 0.7500384052683291003, 0.7650391733736958688, 0.7800399414790623043, 0.7950407095844289618, 0.8100414776897955083, 0.8250422457951620547, 0.8400430139005287122, 0.8550437820058951477, 0.8700445501112619162, 0.8850453182166284627, 0.9000460863219950092, 0.9150468544273615557, 0.9300476225327281021, 0.9450483906380946486, 0.9496006163947603440 ),
 .UNSPECIFIED. ) 
 CURVE ( )  GEOMETRIC_REPRESENTATION_ITEM ( )  RATIONAL_B_SPLINE_CURVE ( ( 0.9433623850486809737, 0.9066821623815489728, 1.000000000000000000, 0.8660254037844387076, 1.000000000000000000, 0.8660254037844387076, 1.000000000000000000, 0.8660254037844387076, 1.000000000000000000, 0.8660254037844387076, 1.000000000000000000, 0.8660254037844387076, 1.000000000000000000, 0.8660254037844387076, 1.000000000000000000, 0.8660254037844387076, 1.000000000000000000, 0.8660254037844387076, 1.000000000000000000, 0.8660254037844387076, 1.000000000000000000, 0.8660254037844387076, 1.000000000000000000, 0.8660254037844387076, 1.000000000000000000, 0.8660254037844387076, 1.000000000000000000, 0.8660254037844387076, 1.000000000000000000, 0.8660254037844387076, 1.000000000000000000, 0.8660254037844387076, 1.000000000000000000, 0.8660254037844387076, 1.000000000000000000, 0.8660254037844387076, 1.000000000000000000, 0.8660254037844387076, 1.000000000000000000, 0.8660254037844387076, 1.000000000000000000, 0.8660254037844387076, 1.000000000000000000, 0.8660254037844387076, 1.000000000000000000, 0.8660254037844387076, 1.000000000000000000, 0.8660254037844387076, 1.000000000000000000, 0.8660254037844387076, 1.000000000000000000, 0.8660254037844387076, 1.000000000000000000, 0.8660254037844387076, 1.000000000000000000, 0.8660254037844387076, 1.000000000000000000, 0.8660254037844387076, 1.000000000000000000, 0.8660254037844387076, 1.000000000000000000, 0.8660254037844387076, 1.000000000000000000, 0.8660254037844387076, 1.000000000000000000, 0.8660254037844387076, 1.000000000000000000, 0.8660254037844387076, 1.000000000000000000, 0.8660254037844387076, 1.000000000000000000, 0.8660254037844387076, 1.000000000000000000, 0.8660254037844387076, 1.000000000000000000, 0.8660254037844387076, 1.000000000000000000, 0.8660254037844387076, 1.000000000000000000, 0.8660254037844387076, 1.000000000000000000, 0.9593432414028746358, 0.9433623850486690943 ) ) 
 REPRESENTATION_ITEM ( '' )  );
#1187 = CARTESIAN_POINT ( 'NONE',  ( -85.40000000000000568, -31.74374999877096926, 99.99999999999998579 ) ) ;
#1188 = CARTESIAN_POINT ( 'NONE',  ( 79.39999999999999147, -32.06250000000000000, -101.7320508075688537 ) ) ;
#1189 = CARTESIAN_POINT ( 'NONE',  ( -3.999999999999999112, 1.539600717838996324, -3.300726591567078039 ) ) ;
#1190 = VECTOR ( 'NONE', #1364, 1000.000000000000000 ) ;
#1191 =( GEOMETRIC_REPRESENTATION_CONTEXT ( 3 ) GLOBAL_UNCERTAINTY_ASSIGNED_CONTEXT ( ( #18445 ) ) GLOBAL_UNIT_ASSIGNED_CONTEXT ( ( #14859, #13397, #18984 ) ) REPRESENTATION_CONTEXT ( 'NONE', 'WORKASPACE' ) );
#1192 = CARTESIAN_POINT ( 'NONE',  ( -81.02178482187500208, -31.00312499938548783, 102.3871387122750889 ) ) ;
#1193 = CARTESIAN_POINT ( 'NONE',  ( -82.39999999999999147, -32.13749999999999574, 103.4641016151377499 ) ) ;
#1194 = DIRECTION ( 'NONE',  ( 1.000000000000000000, 0.000000000000000000, 0.000000000000000000 ) ) ;
#1195 = CARTESIAN_POINT ( 'NONE',  ( 79.64057174634724845, -35.00000000000000000, 99.60353574117782216 ) ) ;
#1196 = CARTESIAN_POINT ( 'NONE',  ( -85.15643035625001289, -34.64062499938548711, 99.99999999999998579 ) ) ;
#1197 = CARTESIAN_POINT ( 'NONE',  ( 233.9782151781249411, -30.89062499938548001, 102.3871387122750889 ) ) ;
#1198 = ORIENTED_EDGE ( 'NONE', *, *, #12336, .T. ) ;
#1199 = CARTESIAN_POINT ( 'NONE',  ( -83.77821517812500929, -32.01562499938548001, -102.3871387122750889 ) ) ;
#1200 = LINE ( 'NONE', #14466, #6177 ) ;
#1201 = VECTOR ( 'NONE', #11469, 1000.000000000000000 ) ;
#1202 = CARTESIAN_POINT ( 'NONE',  ( -80.90000000000000568, -33.39374999877097139, 102.5980762113533018 ) ) ;
#1203 = CARTESIAN_POINT ( 'NONE',  ( 229.8435696437499587, -34.26562499938548001, 101.5914258081833879 ) ) ;
#1204 = CARTESIAN_POINT ( 'NONE',  ( -82.39999999999999147, -31.60312499938548569, 96.81714838363319586 ) ) ;
#1205 = DIRECTION ( 'NONE',  ( 0.000000000000000000, -1.000000000000000000, 0.000000000000000000 ) ) ;
#1206 = CARTESIAN_POINT ( 'NONE',  ( 229.8435696437499871, -31.97812499938548214, -51.59142580818350865 ) ) ;
#1207 = ORIENTED_EDGE ( 'NONE', *, *, #17821, .T. ) ;
#1208 = CARTESIAN_POINT ( 'NONE',  ( -85.15643035624999868, -33.32812499938548001, 98.40857419181659793 ) ) ;
#1209 = CARTESIAN_POINT ( 'NONE',  ( -82.40000000000000568, -30.00000000000000355, -99.99999999999998579 ) ) ;
#1210 = CARTESIAN_POINT ( 'NONE',  ( 83.90000000000000568, -30.52500000000000213, 102.5980762113533018 ) ) ;
#1211 = CARTESIAN_POINT ( 'NONE',  ( -82.40000000000000568, -30.00000000000000355, 103.0000000000000000 ) ) ;
#1212 = AXIS2_PLACEMENT_3D ( 'NONE', #4265, #4552, #19117 ) ;
#1213 = CARTESIAN_POINT ( 'NONE',  ( 231.2217848218749339, -31.41562499938547859, 102.3871387122750889 ) ) ;
#1214 = CARTESIAN_POINT ( 'NONE',  ( 5.599999999999998757, 6.472876824008161592E-16, -5.200000000000001066 ) ) ;
#1215 = CARTESIAN_POINT ( 'NONE',  ( -81.02178482187500208, -35.05312499938548854, 102.3871387122750889 ) ) ;
#1216 = CARTESIAN_POINT ( 'NONE',  ( -79.64356964374998427, -34.04062499938549280, -101.5914258081833879 ) ) ;
#1217 = CARTESIAN_POINT ( 'NONE',  ( 82.39999999999999147, -34.52812499938548996, 96.81714838363319586 ) ) ;
#1218 = CARTESIAN_POINT ( 'NONE',  ( 83.77821517812500929, -33.32812499938548711, -102.3871387122750889 ) ) ;
#1219 = CARTESIAN_POINT ( 'NONE',  ( 229.8435696437499871, -34.60312499938547859, -48.40857419181671162 ) ) ;
#1220 = CARTESIAN_POINT ( 'NONE',  ( -79.64356964374998427, -32.65312499938548285, 101.5914258081833879 ) ) ;
#1221 = CARTESIAN_POINT ( 'NONE',  ( 83.77821517812500929, -30.21562499938548285, -97.61286128772489690 ) ) ;
#1222 = EDGE_LOOP ( 'NONE', ( #8619, #10140 ) ) ;
#1223 = APPLICATION_CONTEXT ( 'automotive_design' ) ;
#1224 = CARTESIAN_POINT ( 'NONE',  ( -82.40000000000000568, -30.00000000000000355, 99.99999999999998579 ) ) ;
#1225 = CARTESIAN_POINT ( 'NONE',  ( 3.806834918298644066, 8.673617379884035472E-16, 3.500000000000000000 ) ) ;
#1226 = CARTESIAN_POINT ( 'NONE',  ( -79.39999999999999147, -32.88750000000000284, 98.26794919243110371 ) ) ;
#1227 = CARTESIAN_POINT ( 'NONE',  ( -85.15643035625001289, -33.74062499938548854, 99.99999999999998579 ) ) ;
#1228 = VERTEX_POINT ( 'NONE', #12501 ) ;
#1229 = CARTESIAN_POINT ( 'NONE',  ( -83.90000000000000568, -33.91874999877096997, 102.5980762113533018 ) ) ;
#1230 = EDGE_CURVE ( 'NONE', #15440, #927, #890, .T. ) ;
#1231 = CARTESIAN_POINT ( 'NONE',  ( 229.8435696437499587, -32.35312499938547859, 101.5914258081833879 ) ) ;
#1232 = CARTESIAN_POINT ( 'NONE',  ( 110.0000000000000000, 10.19999999999997620, -142.6499999999999773 ) ) ;
#1233 = FACE_OUTER_BOUND ( 'NONE', #6066, .T. ) ;
#1234 = EDGE_CURVE ( 'NONE', #13728, #11038, #3167, .T. ) ;
#1235 = EDGE_CURVE ( 'NONE', #18970, #10663, #1963, .T. ) ;
#1236 = CARTESIAN_POINT ( 'NONE',  ( -82.40000000000000568, -30.00000000000000355, 96.99999999999998579 ) ) ;
#1237 = CARTESIAN_POINT ( 'NONE',  ( 234.7546687845693327, -31.99999999999999289, -47.95829548583744639 ) ) ;
#1238 = CARTESIAN_POINT ( 'NONE',  ( -83.77821517812500929, -32.01562499938548001, 97.61286128772489690 ) ) ;
#1239 = CARTESIAN_POINT ( 'NONE',  ( 4.000000000000000000, -2.309401076758514915, -3.433295621305383349 ) ) ;
#1240 = CARTESIAN_POINT ( 'NONE',  ( 79.64356964374999848, -33.62812499938548427, 99.99999999999998579 ) ) ;
#1241 = CARTESIAN_POINT ( 'NONE',  ( 0.2175679805369682140, -1.691499766289325191, 3.500000000000000000 ) ) ;
#1242 = CARTESIAN_POINT ( 'NONE',  ( 229.5999999999999375, -34.89374999877096428, 99.99999999999998579 ) ) ;
#1243 = CARTESIAN_POINT ( 'NONE',  ( 79.64356964374999848, -32.72812499938548569, -99.99999999999998579 ) ) ;
#1244 = CARTESIAN_POINT ( 'NONE',  ( 110.0000000000000000, 10.19999999999997620, -139.9999999999999716 ) ) ;
#1245 = EDGE_LOOP ( 'NONE', ( #6037, #2189, #16909, #7995 ) ) ;
#1246 = CARTESIAN_POINT ( 'NONE',  ( 83.90000000000000568, -32.56874999877096855, 97.40192378864668399 ) ) ;
#1247 = ITEM_DEFINED_TRANSFORMATION ( 'NONE', 'NONE', #13606,  #10540 ) ;
#1248 = CARTESIAN_POINT ( 'NONE',  ( 234.1913891058630099, -35.00000000000002842, -47.72105564972103053 ) ) ;
#1249 = CARTESIAN_POINT ( 'NONE',  ( 233.9782151781249411, -34.60312499938548569, -47.61286128772501769 ) ) ;
#1250 =( BOUNDED_CURVE ( )  B_SPLINE_CURVE ( 2, ( #13241, #10606, #2983, #8939, #5929 ),
 .UNSPECIFIED., .F., .F. ) 
 B_SPLINE_CURVE_WITH_KNOTS ( ( 3, 2, 3 ),
 ( 0.2975293541897477412, 0.3055555555555555802, 0.3125000000000001665 ),
 .UNSPECIFIED. ) 
 CURVE ( )  GEOMETRIC_REPRESENTATION_ITEM ( )  RATIONAL_B_SPLINE_CURVE ( ( 0.9346381638529939195, 0.9225778897267198353, 1.000000000000000000, 0.9330127018922177440, 0.9330127018922194093 ) ) 
 REPRESENTATION_ITEM ( '' )  );
#1251 = EDGE_CURVE ( 'NONE', #11820, #10188, #14419, .T. ) ;
#1252 = DIRECTION ( 'NONE',  ( -1.000000000000000000, 0.000000000000000000, 0.000000000000000000 ) ) ;
#1253 = CARTESIAN_POINT ( 'NONE',  ( -85.31192385480822793, -35.00000000000000711, -100.3932545473404048 ) ) ;
#1254 = ORIENTED_EDGE ( 'NONE', *, *, #2671, .T. ) ;
#1255 = ADVANCED_FACE ( 'NONE', ( #8008 ), #5384, .F. ) ;
#1256 = CARTESIAN_POINT ( 'NONE',  ( -82.39999999999999147, -32.95312499938548711, -103.1828516163667899 ) ) ;
#1257 = EDGE_CURVE ( 'NONE', #4300, #18769, #504, .T. ) ;
#1258 = CARTESIAN_POINT ( 'NONE',  ( -82.40000000000001990, -32.13750000000000284, -97.00000000000000000 ) ) ;
#1259 = ORIENTED_EDGE ( 'NONE', *, *, #5053, .T. ) ;
#1260 = CARTESIAN_POINT ( 'NONE',  ( 81.02178482187500208, -34.90312499938548285, 102.3871387122750889 ) ) ;
#1261 = CARTESIAN_POINT ( 'NONE',  ( -79.64356964375001269, -31.34062499938548640, -101.5914258081833879 ) ) ;
#1262 = DIRECTION ( 'NONE',  ( 1.000000000000000000, 5.337610695313256118E-15, 0.000000000000000000 ) ) ;
#1263 = CARTESIAN_POINT ( 'NONE',  ( -83.90000000000000568, -32.56874999877096855, -97.40192378864668399 ) ) ;
#1264 = CARTESIAN_POINT ( 'NONE',  ( 235.3564303562499447, -32.31562499938547717, 101.5914258081833879 ) ) ;
#1265 = CARTESIAN_POINT ( 'NONE',  ( -79.39999999999999147, -35.11874999877096570, 99.99999999999998579 ) ) ;
#1266 = CARTESIAN_POINT ( 'NONE',  ( -81.02178482187500208, -31.75312499938548427, 97.61286128772489690 ) ) ;
#1267 = CARTESIAN_POINT ( 'NONE',  ( -79.64356964374998427, -32.20312499938548711, -98.40857419181659793 ) ) ;
#1268 = CYLINDRICAL_SURFACE ( 'NONE', #15239, 2.199999999999993516 ) ;
#1269 = CARTESIAN_POINT ( 'NONE',  ( 230.2961164517930968, -35.00002705695778360, 98.07851859032987818 ) ) ;
#1270 = CARTESIAN_POINT ( 'NONE',  ( 83.90000000000000568, -31.36874999877096926, -97.40192378864668399 ) ) ;
#1271 = CARTESIAN_POINT ( 'NONE',  ( 235.5999999999999943, -31.61249999999999716, 101.7320508075688537 ) ) ;
#1272 = VERTEX_POINT ( 'NONE', #607 ) ;
#1273 = CARTESIAN_POINT ( 'NONE',  ( 82.39999999999999147, -34.52812499938548285, -103.1828516163667899 ) ) ;
#1274 = SURFACE_STYLE_USAGE ( .BOTH. , #7318 ) ;
#1275 = CARTESIAN_POINT ( 'NONE',  ( 235.5999999999999943, -32.83124999877095718, 98.26794919243110371 ) ) ;
#1276 = CARTESIAN_POINT ( 'NONE',  ( 229.5999999999999375, -33.54374999877096286, -50.00000000000011369 ) ) ;
#1277 = CARTESIAN_POINT ( 'NONE',  ( -83.77821517812500929, -32.91562499938547859, 97.61286128772489690 ) ) ;
#1278 = ORIENTED_EDGE ( 'NONE', *, *, #15378, .T. ) ;
#1279 = ORIENTED_EDGE ( 'NONE', *, *, #70, .F. ) ;
#1280 = CARTESIAN_POINT ( 'NONE',  ( -82.40000000000000568, -34.38749999999999574, -96.99999999999998579 ) ) ;
#1281 = CARTESIAN_POINT ( 'NONE',  ( -79.83361526238435601, -35.00000000000000711, -98.97827398863965698 ) ) ;
#1282 = CARTESIAN_POINT ( 'NONE',  ( 3.973514160553462737, 3.435084588004189587, -1.181876024140318115 ) ) ;
#1283 = EDGE_LOOP ( 'NONE', ( #1748, #16988, #17522, #18628, #7883 ) ) ;
#1284 = EDGE_CURVE ( 'NONE', #5485, #5649, #1330, .T. ) ;
#1285 = CARTESIAN_POINT ( 'NONE',  ( 3.333333333333335702, -2.694301256218268215, -3.300726591567084256 ) ) ;
#1286 = CARTESIAN_POINT ( 'NONE',  ( 83.90000000000000568, -34.87500000000000000, -102.5980762113533018 ) ) ;
#1287 = ADVANCED_FACE ( 'NONE', ( #12410 ), #17276, .F. ) ;
#1288 = LINE ( 'NONE', #8501, #15479 ) ;
#1289 = CARTESIAN_POINT ( 'NONE',  ( -81.02178482187500208, -30.40312499938548640, 97.61286128772489690 ) ) ;
#1290 = CARTESIAN_POINT ( 'NONE',  ( -83.90000000000000568, -33.07500000000000284, 102.5980762113533018 ) ) ;
#1291 = CARTESIAN_POINT ( 'NONE',  ( 235.4063471324518275, -34.99999999999999289, -50.07101444713918426 ) ) ;
#1292 = DIRECTION ( 'NONE',  ( 0.000000000000000000, 1.000000000000000000, 0.000000000000000000 ) ) ;
#1293 = EDGE_CURVE ( 'NONE', #5861, #5491, #4553, .T. ) ;
#1294 = CARTESIAN_POINT ( 'NONE',  ( 82.40000000000001990, -33.26250000000000284, -97.00000000000000000 ) ) ;
#1295 = CARTESIAN_POINT ( 'NONE',  ( -79.64356964375001269, -34.90312499938548285, 101.5914258081833879 ) ) ;
#1296 = CARTESIAN_POINT ( 'NONE',  ( 229.8435696437499303, -30.14062499938548001, 99.99999999999998579 ) ) ;
#1297 = ORIENTED_EDGE ( 'NONE', *, *, #5113, .F. ) ;
#1298 = CARTESIAN_POINT ( 'NONE',  ( -79.64356964375001269, -30.32812499938548711, -101.5914258081833879 ) ) ;
#1299 = CARTESIAN_POINT ( 'NONE',  ( 232.5999999999999659, -32.58749999999999858, -47.00000000000011369 ) ) ;
#1300 = CARTESIAN_POINT ( 'NONE',  ( 3.973110223768737015, -0.6864646529411585485, -3.565797985667475523 ) ) ;
#1301 =( BOUNDED_CURVE ( )  B_SPLINE_CURVE ( 2, ( #13801, #3645, #3352, #6585, #1987, #534, #9406, #18504, #2084 ),
 .UNSPECIFIED., .F., .F. ) 
 B_SPLINE_CURVE_WITH_KNOTS ( ( 3, 2, 2, 2, 3 ),
 ( 0.5625000000000000000, 0.5694444444444444198, 0.5833333333333333703, 0.5972222222222222099, 0.6041666666666666297 ),
 .UNSPECIFIED. ) 
 CURVE ( )  GEOMETRIC_REPRESENTATION_ITEM ( )  RATIONAL_B_SPLINE_CURVE ( ( 0.9330127018922194093, 0.9330127018922194093, 1.000000000000000000, 0.8660254037844387076, 1.000000000000000000, 0.8660254037844387076, 1.000000000000000000, 0.9330127018922198534, 0.9330127018922192983 ) ) 
 REPRESENTATION_ITEM ( '' )  );
#1302 = DIRECTION ( 'NONE',  ( 1.000000000000000000, -1.387778780781445676E-15, -2.407412430484046130E-31 ) ) ;
#1303 = CARTESIAN_POINT ( 'NONE',  ( -83.77821517812500929, -35.12812499938548427, 102.3871387122750889 ) ) ;
#1304 = DIRECTION ( 'NONE',  ( 0.000000000000000000, 0.000000000000000000, -1.000000000000000000 ) ) ;
#1305 = CARTESIAN_POINT ( 'NONE',  ( 229.8435696437499871, -33.77812499938548285, -51.59142580818350865 ) ) ;
#1306 = ORIENTED_EDGE ( 'NONE', *, *, #10908, .F. ) ;
#1307 = ORIENTED_EDGE ( 'NONE', *, *, #7912, .F. ) ;
#1308 = CARTESIAN_POINT ( 'NONE',  ( 0.2174200650117542322, -2.185595227304859556, 3.214438021527934897 ) ) ;
#1309 = CARTESIAN_POINT ( 'NONE',  ( -82.39999999999999147, -34.97812499938547859, 103.1828516163667899 ) ) ;
#1310 = CARTESIAN_POINT ( 'NONE',  ( 83.20384757729335945, -32.28615380933863577, -97.00000000000000000 ) ) ;
#1311 = CARTESIAN_POINT ( 'NONE',  ( 83.77821517812500929, -35.01562499938548711, 97.61286128772489690 ) ) ;
#1312 = CARTESIAN_POINT ( 'NONE',  ( -83.90000000000000568, -32.62500000000000000, 102.5980762113533018 ) ) ;
#1313 = CARTESIAN_POINT ( 'NONE',  ( 231.2217848218749339, -31.11562499938547788, 97.61286128772489690 ) ) ;
#1314 = CARTESIAN_POINT ( 'NONE',  ( 233.9782151781249411, -34.34062499938547575, -52.38713871227520968 ) ) ;
#1315 = FACE_OUTER_BOUND ( 'NONE', #11332, .T. ) ;
#1316 = CARTESIAN_POINT ( 'NONE',  ( 83.77821517812500929, -33.81562499938548427, 102.3871387122750889 ) ) ;
#1317 = VECTOR ( 'NONE', #9535, 1000.000000000000000 ) ;
#1318 = CARTESIAN_POINT ( 'NONE',  ( 83.77821517812500929, -31.56562499938548427, -97.61286128772489690 ) ) ;
#1319 = CARTESIAN_POINT ( 'NONE',  ( 235.5999999999999943, -30.63749999999999574, -51.73205080756900287 ) ) ;
#1320 = CARTESIAN_POINT ( 'NONE',  ( -85.40000000000000568, -34.08749999999999858, 98.26794919243111792 ) ) ;
#1321 = LINE ( 'NONE', #17248, #5381 ) ;
#1322 = EDGE_LOOP ( 'NONE', ( #17514, #16605, #7351, #5363, #8386 ) ) ;
#1323 = CARTESIAN_POINT ( 'NONE',  ( 79.64356964375001269, -34.49062499938548854, 101.5914258081833879 ) ) ;
#1324 = CARTESIAN_POINT ( 'NONE',  ( 80.90000000000000568, -33.89999999999999858, -102.5980762113533018 ) ) ;
#1325 = CARTESIAN_POINT ( 'NONE',  ( -82.39999999999999147, -32.95312499938548711, 96.81714838363319586 ) ) ;
#1326 = ORIENTED_EDGE ( 'NONE', *, *, #11982, .T. ) ;
#1327 = CARTESIAN_POINT ( 'NONE',  ( -4.211140560182196957, -2.431303136016552013, -3.745885042887436178 ) ) ;
#1328 = EDGE_CURVE ( 'NONE', #7637, #16985, #16283, .T. ) ;
#1329 = AXIS2_PLACEMENT_3D ( 'NONE', #5503, #1292, #12818 ) ;
#1330 = CIRCLE ( 'NONE', #13493, 5.199999999999996625 ) ;
#1332 = CARTESIAN_POINT ( 'NONE',  ( 230.7186334667983658, -32.00000000000000711, 97.98546077809203325 ) ) ;
#1331 =( BOUNDED_CURVE ( )  B_SPLINE_CURVE ( 2, ( #6021, #10319, #7768, #12165, #6310, #16373, #13437, #7481, #15187 ),
 .UNSPECIFIED., .F., .F. ) 
 B_SPLINE_CURVE_WITH_KNOTS ( ( 3, 2, 2, 2, 3 ),
 ( 0.5208333333333333703, 0.5277777777777777901, 0.5416666666666666297, 0.5555555555555555802, 0.5625000000000000000 ),
 .UNSPECIFIED. ) 
 CURVE ( )  GEOMETRIC_REPRESENTATION_ITEM ( )  RATIONAL_B_SPLINE_CURVE ( ( 0.9330127018922192983, 0.9330127018922198534, 1.000000000000000000, 0.8660254037844387076, 1.000000000000000000, 0.8660254037844387076, 1.000000000000000000, 0.9330127018922194093, 0.9330127018922194093 ) ) 
 REPRESENTATION_ITEM ( '' )  );
#1333 = DIRECTION ( 'NONE',  ( -1.387778780781445478E-15, -1.000000000000000000, -1.214306433183764966E-16 ) ) ;
#1334 = CARTESIAN_POINT ( 'NONE',  ( -85.40000000000000568, -33.63356250001229597, 98.26794919243111792 ) ) ;
#1335 = CARTESIAN_POINT ( 'NONE',  ( -82.40000000000001990, -33.26250000000000284, -103.0000000000000000 ) ) ;
#1336 = CARTESIAN_POINT ( 'NONE',  ( -82.39999999999999147, -32.81250000000000000, -103.0000000000000000 ) ) ;
#1337 = CARTESIAN_POINT ( 'NONE',  ( -85.15643035625001289, -31.94062499938548427, 99.99999999999998579 ) ) ;
#1338 = CARTESIAN_POINT ( 'NONE',  ( 230.5871892821561460, -32.00000000000002132, 98.10821574224502228 ) ) ;
#1339 = CARTESIAN_POINT ( 'NONE',  ( 81.02178482187500208, -33.70312499938548711, 97.61286128772489690 ) ) ;
#1340 = CARTESIAN_POINT ( 'NONE',  ( -83.20384757729335945, -32.60759618943233562, 102.9999999999999858 ) ) ;
#1341 = CARTESIAN_POINT ( 'NONE',  ( -81.59615242270662350, -32.56740381056766864, -97.00000000000000000 ) ) ;
#1342 = CARTESIAN_POINT ( 'NONE',  ( 83.77821517812500929, -33.77812499938548285, -102.3871387122750889 ) ) ;
#1343 = CARTESIAN_POINT ( 'NONE',  ( -85.15643035625001289, -32.05312499938548854, -99.99999999999998579 ) ) ;
#1344 = VECTOR ( 'NONE', #12767, 1000.000000000000000 ) ;
#1345 = ORIENTED_EDGE ( 'NONE', *, *, #5809, .T. ) ;
#1346 = CARTESIAN_POINT ( 'NONE',  ( 82.39999999999999147, -33.20624999877097139, 103.4641016151377499 ) ) ;
#1347 = CONTEXT_DEPENDENT_SHAPE_REPRESENTATION ( #2214, #15761 ) ;
#1348 = LINE ( 'NONE', #13249, #3675 ) ;
#1349 = DIRECTION ( 'NONE',  ( 0.000000000000000000, 0.000000000000000000, -1.000000000000000000 ) ) ;
#1350 = EDGE_CURVE ( 'NONE', #4990, #15743, #6857, .T. ) ;
#1351 = CARTESIAN_POINT ( 'NONE',  ( -79.64356964375001269, -30.44062499938548783, 98.40857419181659793 ) ) ;
#1352 = CARTESIAN_POINT ( 'NONE',  ( 232.5999999999999375, -29.99999999999999645, -50.00000000000011369 ) ) ;
#1353 = ORIENTED_EDGE ( 'NONE', *, *, #4995, .T. ) ;
#1354 = CARTESIAN_POINT ( 'NONE',  ( -84.51155491706698797, -35.14114833091483803, -101.7717912238936719 ) ) ;
#1355 = CARTESIAN_POINT ( 'NONE',  ( 4.000000000000000000, 1.680228229147133767, -3.316631783032546021 ) ) ;
#1356 = VERTEX_POINT ( 'NONE', #16575 ) ;
#1357 = CARTESIAN_POINT ( 'NONE',  ( -79.64356964375001269, -34.49062499938548854, -101.5914258081833879 ) ) ;
#1358 = LINE ( 'NONE', #16493, #4568 ) ;
#1359 = CARTESIAN_POINT ( 'NONE',  ( -80.90000000000000568, -31.59374999877097423, -97.40192378864668399 ) ) ;
#1360 = CARTESIAN_POINT ( 'NONE',  ( 229.8435696437499871, -31.64062499938547290, 98.40857419181659793 ) ) ;
#1361 = CARTESIAN_POINT ( 'NONE',  ( -82.39999999999999147, -33.65624999877096712, 96.53589838486223584 ) ) ;
#1362 = CARTESIAN_POINT ( 'NONE',  ( -81.02178482187500208, -32.80312499938548854, 102.3871387122750889 ) ) ;
#1363 = CARTESIAN_POINT ( 'NONE',  ( -79.64356964374998427, -34.37812499938548427, -101.5914258081833879 ) ) ;
#1364 = DIRECTION ( 'NONE',  ( -0.000000000000000000, -1.000000000000000000, -0.000000000000000000 ) ) ;
#1365 = ADVANCED_FACE ( 'NONE', ( #3175 ), #10413, .T. ) ;
#1366 = FACE_OUTER_BOUND ( 'NONE', #1874, .T. ) ;
#1367 = CARTESIAN_POINT ( 'NONE',  ( 79.39999999999999147, -31.93124999877096926, -98.26794919243110371 ) ) ;
#1368 = CARTESIAN_POINT ( 'NONE',  ( 229.5999999999999375, -34.49999999999999289, 99.99999999999998579 ) ) ;
#1369 =( BOUNDED_CURVE ( )  B_SPLINE_CURVE ( 2, ( #8416, #19166, #3922, #2639, #4118, #10080, #12912, #5407, #14368 ),
 .UNSPECIFIED., .F., .F. ) 
 B_SPLINE_CURVE_WITH_KNOTS ( ( 3, 2, 2, 2, 3 ),
 ( 0.8541666666666665186, 0.8611111111111111605, 0.8750000000000000000, 0.8888888888888888395, 0.8958333333333333703 ),
 .UNSPECIFIED. ) 
 CURVE ( )  GEOMETRIC_REPRESENTATION_ITEM ( )  RATIONAL_B_SPLINE_CURVE ( ( 0.9330127018922194093, 0.9330127018922177440, 1.000000000000000000, 0.8660254037844387076, 1.000000000000000000, 0.8660254037844387076, 1.000000000000000000, 0.9330127018922187432, 0.9330127018922192983 ) ) 
 REPRESENTATION_ITEM ( '' )  );
#1370 = VERTEX_POINT ( 'NONE', #1536 ) ;
#1371 = CARTESIAN_POINT ( 'NONE',  ( 81.02178482187500208, -34.94062499938548427, -102.3871387122750889 ) ) ;
#1372 = CARTESIAN_POINT ( 'NONE',  ( 234.0999999999999375, -33.84374999877096002, 102.5980762113533018 ) ) ;
#1373 = CARTESIAN_POINT ( 'NONE',  ( 231.0999999999999375, -33.61874999877096570, -52.59807621135342970 ) ) ;
#1374 = EDGE_CURVE ( 'NONE', #4798, #17054, #1186, .T. ) ;
#1375 = CARTESIAN_POINT ( 'NONE',  ( -82.39999999999999147, -32.50312499938548427, 96.81714838363319586 ) ) ;
#1376 = ORIENTED_EDGE ( 'NONE', *, *, #12861, .T. ) ;
#1377 = ORIENTED_EDGE ( 'NONE', *, *, #4747, .T. ) ;
#1378 = CARTESIAN_POINT ( 'NONE',  ( -83.92761994969268358, -32.00000000000000000, 97.66884955414403180 ) ) ;
#1379 = CARTESIAN_POINT ( 'NONE',  ( 229.5999999999999091, -34.97364041986482164, 98.90809577818235709 ) ) ;
#1380 = CARTESIAN_POINT ( 'NONE',  ( 4.050823680195224874, 3.779313952391379683, -0.5899027668435159466 ) ) ;
#1381 = EDGE_LOOP ( 'NONE', ( #9993, #4042, #14838, #7130 ) ) ;
#1382 = CARTESIAN_POINT ( 'NONE',  ( -82.32247963938031887, -35.00000000000000000, 102.7610832838413444 ) ) ;
#1383 = CARTESIAN_POINT ( 'NONE',  ( 82.39999999999999147, -34.16250000000000142, -96.53589838486223584 ) ) ;
#1384 = LINE ( 'NONE', #3919, #4252 ) ;
#1385 = CARTESIAN_POINT ( 'NONE',  ( -79.64356964374999848, -34.07812499938548711, 99.99999999999998579 ) ) ;
#1386 = CARTESIAN_POINT ( 'NONE',  ( -85.40000000000000568, -32.70000000000000284, 99.99999999999998579 ) ) ;
#1387 = CARTESIAN_POINT ( 'NONE',  ( -83.90000000000000568, -31.81874999877096855, 97.40192378864668399 ) ) ;
#1388 = DIRECTION ( 'NONE',  ( 1.000000000000000000, 0.000000000000000000, -0.000000000000000000 ) ) ;
#1389 = CARTESIAN_POINT ( 'NONE',  ( -84.69814161231457206, -35.29583579514545733, 98.07164704222797980 ) ) ;
#1390 = CARTESIAN_POINT ( 'NONE',  ( 105.1999999999999744, -31.99999999999999289, 150.0000000000000000 ) ) ;
#1391 = VERTEX_POINT ( 'NONE', #8255 ) ;
#1392 = SHAPE_REPRESENTATION_RELATIONSHIP ( 'NONE' , 'NONE' ,  #406, #5334 ) ;
#1393 = CARTESIAN_POINT ( 'NONE',  ( -85.15643035624999868, -31.07812499938548356, -101.5914258081833879 ) ) ;
#1394 = LINE ( 'NONE', #3134, #18639 ) ;
#1395 = CARTESIAN_POINT ( 'NONE',  ( -82.39999999999999147, -30.78750000000000142, 102.9999999999999858 ) ) ;
#1396 = CARTESIAN_POINT ( 'NONE',  ( -82.39999999999999147, -30.92812499938548143, 103.1828516163667899 ) ) ;
#1397 = CARTESIAN_POINT ( 'NONE',  ( 232.5999999999999375, -32.95312499938548001, -53.18285161636690361 ) ) ;
#1398 = ORIENTED_EDGE ( 'NONE', *, *, #4541, .F. ) ;
#1399 = ORIENTED_EDGE ( 'NONE', *, *, #3870, .F. ) ;
#1400 = CARTESIAN_POINT ( 'NONE',  ( 0.000000000000000000, -3.031088913245531202, 1.750000000000006661 ) ) ;
#1401 = EDGE_CURVE ( 'NONE', #15307, #16462, #2539, .T. ) ;
#1402 = CARTESIAN_POINT ( 'NONE',  ( -82.39999999999999147, -32.13749999999999574, 103.4641016151377499 ) ) ;
#1403 = CARTESIAN_POINT ( 'NONE',  ( -85.40000000000000568, -32.15624999877096712, 101.7320508075688679 ) ) ;
#1404 = CARTESIAN_POINT ( 'NONE',  ( 85.40000000000000568, -30.48749999999999716, 101.7320508075688679 ) ) ;
#1405 = CARTESIAN_POINT ( 'NONE',  ( -82.40000000000001990, -31.68750000000000711, 103.0000000000000000 ) ) ;
#1406 = CARTESIAN_POINT ( 'NONE',  ( 229.8435696437499871, -31.45312499938547290, 101.5914258081833879 ) ) ;
#1407 = CARTESIAN_POINT ( 'NONE',  ( 232.9413037568956497, -34.96883842999723413, -47.01420019955246943 ) ) ;
#1408 = CARTESIAN_POINT ( 'NONE',  ( 85.15643035625001289, -34.19062499938548427, 99.99999999999998579 ) ) ;
#1409 = CARTESIAN_POINT ( 'NONE',  ( 83.77821517812500929, -32.01562499938548001, -97.61286128772489690 ) ) ;
#1410 =( BOUNDED_CURVE ( )  B_SPLINE_CURVE ( 2, ( #17115, #5399, #8408, #996, #12710, #18873, #5300, #11342, #17307 ),
 .UNSPECIFIED., .F., .F. ) 
 B_SPLINE_CURVE_WITH_KNOTS ( ( 3, 2, 2, 2, 3 ),
 ( 0.4791666666666666852, 0.4861111111111111049, 0.5000000000000000000, 0.5138888888888888395, 0.5208333333333331483 ),
 .UNSPECIFIED. ) 
 CURVE ( )  GEOMETRIC_REPRESENTATION_ITEM ( )  RATIONAL_B_SPLINE_CURVE ( ( 0.9330127018922194093, 0.9330127018922196314, 1.000000000000000000, 0.8660254037844387076, 1.000000000000000000, 0.8660254037844387076, 1.000000000000000000, 0.9330127018922209636, 0.9330127018922194093 ) ) 
 REPRESENTATION_ITEM ( '' )  );
#1411 = CARTESIAN_POINT ( 'NONE',  ( 234.0999999999999375, -31.19999999999999574, -47.40192378864679768 ) ) ;
#1412 = CARTESIAN_POINT ( 'NONE',  ( -85.15643035625001289, -34.64062499938548711, 99.99999999999998579 ) ) ;
#1413 = CARTESIAN_POINT ( 'NONE',  ( 83.77821517812500929, -32.91562499938547859, -97.61286128772489690 ) ) ;
#1414 = ORIENTED_EDGE ( 'NONE', *, *, #18431, .F. ) ;
#1415 = DIRECTION ( 'NONE',  ( 0.000000000000000000, -1.000000000000000000, 0.000000000000000000 ) ) ;
#1416 = CARTESIAN_POINT ( 'NONE',  ( -79.39999999999999147, -34.70624999877097139, 101.7320508075688537 ) ) ;
#1417 = CARTESIAN_POINT ( 'NONE',  ( 233.9782151781249411, -31.30312499938547788, -52.38713871227520968 ) ) ;
#1418 =( BOUNDED_CURVE ( )  B_SPLINE_CURVE ( 2, ( #15673, #15769, #12741, #7856, #9413, #12539, #15380, #16945, #18611 ),
 .UNSPECIFIED., .F., .F. ) 
 B_SPLINE_CURVE_WITH_KNOTS ( ( 3, 2, 2, 2, 3 ),
 ( 0.7708333333333331483, 0.7777777777777777901, 0.7916666666666666297, 0.8055555555555555802, 0.8125000000000001110 ),
 .UNSPECIFIED. ) 
 CURVE ( )  GEOMETRIC_REPRESENTATION_ITEM ( )  RATIONAL_B_SPLINE_CURVE ( ( 0.9330127018922194093, 0.9330127018922177440, 1.000000000000000000, 0.8660254037844387076, 1.000000000000000000, 0.8660254037844387076, 1.000000000000000000, 0.9330127018922182991, 0.9330127018922194093 ) ) 
 REPRESENTATION_ITEM ( '' )  );
#1419 = CARTESIAN_POINT ( 'NONE',  ( -79.64356964374999848, -33.06562499938548427, 99.99999999999998579 ) ) ;
#1420 = EDGE_LOOP ( 'NONE', ( #1182, #9956, #9327, #15515 ) ) ;
#1421 = CARTESIAN_POINT ( 'NONE',  ( -83.90000000000000568, -34.06874999877096855, 97.40192378864668399 ) ) ;
#1422 = CARTESIAN_POINT ( 'NONE',  ( 1.411581201560190495E-15, 4.862606272033091592, -3.745885042887436622 ) ) ;
#1423 = DIRECTION ( 'NONE',  ( 0.000000000000000000, -1.000000000000000000, 0.000000000000000000 ) ) ;
#1424 = CARTESIAN_POINT ( 'NONE',  ( -80.90000000000000568, -32.39606250001229881, 97.40192378864668399 ) ) ;
#1425 = CARTESIAN_POINT ( 'NONE',  ( -82.40000000000001990, -32.08124999877097139, -97.00000000000000000 ) ) ;
#1426 = DIRECTION ( 'NONE',  ( 0.000000000000000000, 0.000000000000000000, 1.000000000000000000 ) ) ;
#1427 = CARTESIAN_POINT ( 'NONE',  ( -79.64356964374999848, -32.16562499938548569, 99.99999999999998579 ) ) ;
#1428 = CARTESIAN_POINT ( 'NONE',  ( 84.53225329756209305, -31.99999999999999289, 101.7559005160108256 ) ) ;
#1429 = CARTESIAN_POINT ( 'NONE',  ( 79.64356964374999848, -31.82812499938548356, 99.99999999999998579 ) ) ;
#1430 = DIRECTION ( 'NONE',  ( 0.000000000000000000, 1.000000000000000000, 0.000000000000000000 ) ) ;
#1431 = CARTESIAN_POINT ( 'NONE',  ( -85.16931825408420309, -31.99999999999998579, -99.76128878215617135 ) ) ;
#1432 = CARTESIAN_POINT ( 'NONE',  ( -83.77821517812500929, -30.32812499938548711, -102.3871387122750889 ) ) ;
#1433 = ORIENTED_EDGE ( 'NONE', *, *, #7219, .F. ) ;
#1434 = CARTESIAN_POINT ( 'NONE',  ( 85.40000000000000568, -34.48124999877096997, 101.7320508075688679 ) ) ;
#1435 = DIRECTION ( 'NONE',  ( 0.000000000000000000, 0.000000000000000000, 1.000000000000000000 ) ) ;
#1436 = CARTESIAN_POINT ( 'NONE',  ( 235.3564303562499447, -35.01562499938548001, -48.40857419181671162 ) ) ;
#1437 = CARTESIAN_POINT ( 'NONE',  ( -85.15643035624999868, -30.74062499938548143, 98.40857419181659793 ) ) ;
#1438 =( BOUNDED_CURVE ( )  B_SPLINE_CURVE ( 2, ( #16800, #7900, #18171, #3212, #17981, #6256, #12109, #12397, #3501 ),
 .UNSPECIFIED., .F., .F. ) 
 B_SPLINE_CURVE_WITH_KNOTS ( ( 3, 2, 2, 2, 3 ),
 ( 0.3958333333333333703, 0.4027777777777777901, 0.4166666666666666852, 0.4305555555555555802, 0.4375000000000001110 ),
 .UNSPECIFIED. ) 
 CURVE ( )  GEOMETRIC_REPRESENTATION_ITEM ( )  RATIONAL_B_SPLINE_CURVE ( ( 0.9330127018922194093, 0.9330127018922196314, 1.000000000000000000, 0.8660254037844387076, 1.000000000000000000, 0.8660254037844387076, 1.000000000000000000, 0.9330127018922182991, 0.9330127018922194093 ) ) 
 REPRESENTATION_ITEM ( '' )  );
#1439 = CARTESIAN_POINT ( 'NONE',  ( 79.68063642056725371, -32.00000000000002132, 101.2652131118146741 ) ) ;
#1440 = ORIENTED_EDGE ( 'NONE', *, *, #15000, .F. ) ;
#1441 = CARTESIAN_POINT ( 'NONE',  ( -83.77821517812500929, -34.26562499938548711, -102.3871387122750889 ) ) ;
#1442 = CARTESIAN_POINT ( 'NONE',  ( 4.211405965630455661, 2.460463115436283932, -3.751298928144577882 ) ) ;
#1443 = FACE_OUTER_BOUND ( 'NONE', #7708, .T. ) ;
#1444 = CARTESIAN_POINT ( 'NONE',  ( -79.64356964374999848, -32.72812499938548569, -99.99999999999998579 ) ) ;
#1445 = CIRCLE ( 'NONE', #16413, 6.000000000000015987 ) ;
#1446 = CARTESIAN_POINT ( 'NONE',  ( 109.9999999999999716, -14.00063509461108247, 8.083270440699362069 ) ) ;
#1447 = CARTESIAN_POINT ( 'NONE',  ( -83.90000000000000568, -30.76874999877097139, -97.40192378864668399 ) ) ;
#1448 = ADVANCED_FACE ( 'NONE', ( #2872 ), #1609, .F. ) ;
#1449 = CARTESIAN_POINT ( 'NONE',  ( 229.8435696437499303, -30.70312499938548001, 99.99999999999998579 ) ) ;
#1450 = CARTESIAN_POINT ( 'NONE',  ( -80.90000000000000568, -31.59768749875868110, 102.5980762113533018 ) ) ;
#1451 = CARTESIAN_POINT ( 'NONE',  ( -85.15643035625001289, -32.50312499938548427, 99.99999999999998579 ) ) ;
#1452 = CARTESIAN_POINT ( 'NONE',  ( -85.15643035625001289, -34.67812499938548143, -101.5914258081833879 ) ) ;
#1453 = CARTESIAN_POINT ( 'NONE',  ( 82.39999999999999147, -34.07812499938548711, 96.81714838363319586 ) ) ;
#1454 = CARTESIAN_POINT ( 'NONE',  ( 111.0000000000000000, 10.19999999999997620, -139.9999999999999716 ) ) ;
#1455 = CARTESIAN_POINT ( 'NONE',  ( -84.51155153715826884, -35.14114847181267720, 98.22820474807231506 ) ) ;
#1456 = CARTESIAN_POINT ( 'NONE',  ( 83.90000000000000568, -34.06874999877096855, -97.40192378864668399 ) ) ;
#1457 = CARTESIAN_POINT ( 'NONE',  ( 234.0999999999999375, -33.29999999999999716, 97.40192378864668399 ) ) ;
#1458 = ORIENTED_EDGE ( 'NONE', *, *, #16123, .T. ) ;
#1459 = CARTESIAN_POINT ( 'NONE',  ( 79.64356964374999848, -34.86562499938548143, -99.99999999999998579 ) ) ;
#1460 =( NAMED_UNIT ( * ) SI_UNIT ( $, .STERADIAN. ) SOLID_ANGLE_UNIT ( ) );
#1461 = CARTESIAN_POINT ( 'NONE',  ( 233.9782151781249411, -31.00312499938548072, 102.3871387122750889 ) ) ;
#1462 = CARTESIAN_POINT ( 'NONE',  ( 231.0999999999999375, -33.01874999877096428, -47.40192378864679768 ) ) ;
#1463 = CARTESIAN_POINT ( 'NONE',  ( -82.39999999999999147, -33.85312499938548569, 96.81714838363319586 ) ) ;
#1464 = EDGE_LOOP ( 'NONE', ( #11747, #11309, #16868, #7244 ) ) ;
#1465 = ORIENTED_EDGE ( 'NONE', *, *, #18460, .T. ) ;
#1466 = CARTESIAN_POINT ( 'NONE',  ( -79.39999999999999147, -34.27499999999999858, -99.99999999999998579 ) ) ;
#1467 = CARTESIAN_POINT ( 'NONE',  ( 4.180345472528542494, 2.086001522971433264, 3.570468649087212398 ) ) ;
#1468 = CARTESIAN_POINT ( 'NONE',  ( 0.000000000000000000, 0.000000000000000000, -5.000000000000000000 ) ) ;
#1469 = ORIENTED_EDGE ( 'NONE', *, *, #10312, .F. ) ;
#1470 = CARTESIAN_POINT ( 'NONE',  ( -83.03192786677307424, -35.00000000000000711, 102.6890373435400221 ) ) ;
#1471 = AXIS2_PLACEMENT_3D ( 'NONE', #17709, #7632, #14965 ) ;
#1472 = CYLINDRICAL_SURFACE ( 'NONE', #10483, 3.000000000000002665 ) ;
#1473 = CARTESIAN_POINT ( 'NONE',  ( -83.77821517812500929, -34.37812499938548427, 97.61286128772489690 ) ) ;
#1474 = CARTESIAN_POINT ( 'NONE',  ( -80.90000000000000568, -30.69374999877097210, 102.5980762113533018 ) ) ;
#1475 = CARTESIAN_POINT ( 'NONE',  ( -82.39999999999999147, -30.50624999877097210, 96.53589838486223584 ) ) ;
#1476 = AXIS2_PLACEMENT_3D ( 'NONE', #15312, #674, #18638 ) ;
#1477 = FACE_OUTER_BOUND ( 'NONE', #16511, .T. ) ;
#1478 =( BOUNDED_CURVE ( )  B_SPLINE_CURVE ( 2, ( #3477, #13738, #4566, #16491, #6233, #7784, #6420, #1824, #1726 ),
 .UNSPECIFIED., .F., .F. ) 
 B_SPLINE_CURVE_WITH_KNOTS ( ( 3, 2, 2, 2, 3 ),
 ( 0.6041666666666666297, 0.6111111111111111605, 0.6250000000000000000, 0.6388888888888888395, 0.6458333333333333703 ),
 .UNSPECIFIED. ) 
 CURVE ( )  GEOMETRIC_REPRESENTATION_ITEM ( )  RATIONAL_B_SPLINE_CURVE ( ( 0.9330127018922192983, 0.9330127018922187432, 1.000000000000000000, 0.8660254037844387076, 1.000000000000000000, 0.8660254037844387076, 1.000000000000000000, 0.9330127018922187432, 0.9330127018922192983 ) ) 
 REPRESENTATION_ITEM ( '' )  );
#1479 = EDGE_CURVE ( 'NONE', #16118, #14240, #2651, .T. ) ;
#1480 = CARTESIAN_POINT ( 'NONE',  ( 4.158806965674306078, 1.986429158307092768, 3.559403772175832259 ) ) ;
#1481 = LINE ( 'NONE', #1390, #9928 ) ;
#1482 = B_SPLINE_CURVE_WITH_KNOTS ( 'NONE', 3,
 ( #9096, #15155, #16722, #12324, #18290, #3329, #12419, #1772 ),
 .UNSPECIFIED., .F., .F.,
 ( 4, 2, 2, 4 ),
 ( 0.005725059856848645212, 0.006314084072593634418, 0.006903108288338624492, 0.008081156719828603771 ),
 .UNSPECIFIED. ) ;
#1483 = CARTESIAN_POINT ( 'NONE',  ( -85.40000000000000568, -34.48124999877096997, -101.7320508075688821 ) ) ;
#1484 = EDGE_LOOP ( 'NONE', ( #2751, #15911, #9153, #14334 ) ) ;
#1485 = AXIS2_PLACEMENT_3D ( 'NONE', #921, #15952, #5695 ) ;
#1486 =( NAMED_UNIT ( * ) PLANE_ANGLE_UNIT ( ) SI_UNIT ( $, .RADIAN. ) );
#1487 = CARTESIAN_POINT ( 'NONE',  ( -85.15643035625001289, -34.19062499938548427, -99.99999999999998579 ) ) ;
#1488 = LINE ( 'NONE', #7441, #11783 ) ;
#1489 = CARTESIAN_POINT ( 'NONE',  ( 96.99999999999994316, -29.80000000000000426, 150.0000000000000000 ) ) ;
#1490 = CARTESIAN_POINT ( 'NONE',  ( 3.973110223767137850, 2.263313079739336463E-11, 3.565797985667434222 ) ) ;
#1491 = CARTESIAN_POINT ( 'NONE',  ( -79.64356964375001269, -32.20312499938548001, 101.5914258081833879 ) ) ;
#1492 = DIRECTION ( 'NONE',  ( 0.000000000000000000, -1.000000000000000000, 0.000000000000000000 ) ) ;
#1493 = CARTESIAN_POINT ( 'NONE',  ( 235.3564303562499447, -33.55312499938548143, -48.40857419181671162 ) ) ;
#1494 = VECTOR ( 'NONE', #15806, 1000.000000000000000 ) ;
#1495 = MECHANICAL_DESIGN_GEOMETRIC_PRESENTATION_REPRESENTATION (  '', ( #2115 ), #14585 ) ;
#1497 = EDGE_CURVE ( 'NONE', #4468, #592, #11900, .T. ) ;
#1496 = ORIENTED_EDGE ( 'NONE', *, *, #6126, .T. ) ;
#1498 = VERTEX_POINT ( 'NONE', #7268 ) ;
#1499 = CARTESIAN_POINT ( 'NONE',  ( -85.40000000000000568, -32.25000000000000000, 99.99999999999998579 ) ) ;
#1500 = EDGE_CURVE ( 'NONE', #484, #2622, #14883, .T. ) ;
#1501 = CARTESIAN_POINT ( 'NONE',  ( -79.39999999999999147, -32.41874999877096997, 99.99999999999998579 ) ) ;
#1502 = CARTESIAN_POINT ( 'NONE',  ( 85.40000000000000568, -33.18750000000000000, 101.7320508075688679 ) ) ;
#1503 = VECTOR ( 'NONE', #6129, 1000.000000000000000 ) ;
#1504 = CARTESIAN_POINT ( 'NONE',  ( -4.000000000000003553, 2.309401076758496263, -3.504269196027868905 ) ) ;
#1505 = CARTESIAN_POINT ( 'NONE',  ( 235.3564303562499447, -33.10312499938547859, 101.5914258081833879 ) ) ;
#1506 = CARTESIAN_POINT ( 'NONE',  ( 235.3564303562499447, -33.92812499938548143, -51.59142580818350154 ) ) ;
#1507 = CIRCLE ( 'NONE', #6500, 2.500000000000000444 ) ;
#1508 = AXIS2_PLACEMENT_3D ( 'NONE', #9648, #2018, #10720 ) ;
#1509 = CARTESIAN_POINT ( 'NONE',  ( 79.64356964374999848, -30.36562499938548498, -99.99999999999998579 ) ) ;
#1510 = VERTEX_POINT ( 'NONE', #52 ) ;
#1511 = EDGE_CURVE ( 'NONE', #2507, #16323, #4665, .T. ) ;
#1512 = CARTESIAN_POINT ( 'NONE',  ( 235.5999999999999943, -30.71249999999999858, -48.26794919243124582 ) ) ;
#1513 = CARTESIAN_POINT ( 'NONE',  ( 84.70388354820684640, -35.00002705695777649, -98.07851859032987818 ) ) ;
#1514 = CARTESIAN_POINT ( 'NONE',  ( 85.15643035624999868, -33.25312499938548427, -101.5914258081833879 ) ) ;
#1515 = ORIENTED_EDGE ( 'NONE', *, *, #11295, .T. ) ;
#1516 = CARTESIAN_POINT ( 'NONE',  ( 232.5999999999999375, -34.33124999877097139, -47.00000000000011369 ) ) ;
#1517 = AXIS2_PLACEMENT_3D ( 'NONE', #3863, #9825, #14312 ) ;
#1518 = CARTESIAN_POINT ( 'NONE',  ( 79.39999999999999147, -33.86250000000000426, -101.7320508075688537 ) ) ;
#1519 = CARTESIAN_POINT ( 'NONE',  ( 229.8435696437499871, -31.56562499938547717, -48.40857419181671162 ) ) ;
#1520 = CARTESIAN_POINT ( 'NONE',  ( -83.77821517812500929, -34.56562499938548427, 102.3871387122750889 ) ) ;
#1521 = ORIENTED_EDGE ( 'NONE', *, *, #7205, .T. ) ;
#1522 = CARTESIAN_POINT ( 'NONE',  ( -3.999999999999999112, -2.309401076758512694, -3.504269196027871125 ) ) ;
#1523 = AXIS2_PLACEMENT_3D ( 'NONE', #345, #18698, #6679 ) ;
#1524 = CARTESIAN_POINT ( 'NONE',  ( -82.40000000000000568, -30.95624999877097139, 96.99999999999998579 ) ) ;
#1525 = CARTESIAN_POINT ( 'NONE',  ( 85.15643035625001289, -31.04062499938548569, 99.99999999999998579 ) ) ;
#1526 = CARTESIAN_POINT ( 'NONE',  ( -83.90000000000000568, -32.77106250001229171, 97.40192378864668399 ) ) ;
#1527 = ADVANCED_FACE ( 'NONE', ( #7557 ), #13514, .F. ) ;
#1528 = CARTESIAN_POINT ( 'NONE',  ( -99.99999999999998579, -5.200000000000000178, -150.0000000000000000 ) ) ;
#1529 = CARTESIAN_POINT ( 'NONE',  ( -82.39999999999999147, -32.36250000000000426, 96.99999999999997158 ) ) ;
#1530 = CARTESIAN_POINT ( 'NONE',  ( -79.64356964375001269, -30.85312499938548569, 101.5914258081833879 ) ) ;
#1531 = CARTESIAN_POINT ( 'NONE',  ( 85.03799702444359809, -32.00000000000000000, 100.8187845449565572 ) ) ;
#1532 = CARTESIAN_POINT ( 'NONE',  ( 79.64356964375001269, -31.79062499938548569, 101.5914258081833879 ) ) ;
#1533 = CARTESIAN_POINT ( 'NONE',  ( -82.40000000000000568, -30.00000000000000355, -96.99999999999998579 ) ) ;
#1534 = EDGE_CURVE ( 'NONE', #3915, #18169, #9388, .T. ) ;
#1535 = DIRECTION ( 'NONE',  ( 0.000000000000000000, 0.000000000000000000, -1.000000000000000000 ) ) ;
#1536 = CARTESIAN_POINT ( 'NONE',  ( 232.5999999999999091, -34.10624999877096286, -53.00000000000010658 ) ) ;
#1537 = CARTESIAN_POINT ( 'NONE',  ( -81.02178482187500208, -30.40312499938548640, -102.3871387122750889 ) ) ;
#1538 =( BOUNDED_CURVE ( )  B_SPLINE_CURVE ( 2, ( #16992, #4802, #3314, #13857, #15532, #12495, #13768, #9271, #408 ),
 .UNSPECIFIED., .F., .F. ) 
 B_SPLINE_CURVE_WITH_KNOTS ( ( 3, 2, 2, 2, 3 ),
 ( 0.6875000000000000000, 0.6944444444444444198, 0.7083333333333333703, 0.7222222222222222099, 0.7291666666666668517 ),
 .UNSPECIFIED. ) 
 CURVE ( )  GEOMETRIC_REPRESENTATION_ITEM ( )  RATIONAL_B_SPLINE_CURVE ( ( 0.9330127018922194093, 0.9330127018922194093, 1.000000000000000000, 0.8660254037844387076, 1.000000000000000000, 0.8660254037844387076, 1.000000000000000000, 0.9330127018922177440, 0.9330127018922194093 ) ) 
 REPRESENTATION_ITEM ( '' )  );
#1539 = ORIENTED_EDGE ( 'NONE', *, *, #14831, .T. ) ;
#1540 = CARTESIAN_POINT ( 'NONE',  ( 79.64356964374999848, -31.37812499938548427, 99.99999999999998579 ) ) ;
#1541 = DIRECTION ( 'NONE',  ( -0.000000000000000000, -0.000000000000000000, -1.000000000000000000 ) ) ;
#1542 = FACE_OUTER_BOUND ( 'NONE', #2026, .T. ) ;
#1543 = CARTESIAN_POINT ( 'NONE',  ( 4.175572532730931208, -2.061029303918061828, -3.569807470274388717 ) ) ;
#1544 = CARTESIAN_POINT ( 'NONE',  ( -79.64356964375001269, -31.86562499938548143, 101.5914258081833879 ) ) ;
#1545 = LINE ( 'NONE', #16292, #10244 ) ;
#1546 = VERTEX_POINT ( 'NONE', #15734 ) ;
#1547 = CARTESIAN_POINT ( 'NONE',  ( -79.39999999999999147, -30.63750000000000284, -101.7320508075688821 ) ) ;
#1548 = CARTESIAN_POINT ( 'NONE',  ( 4.000000000000000888, -0.8578082829538523635, -3.433262215449808696 ) ) ;
#1549 = CARTESIAN_POINT ( 'NONE',  ( -85.40000000000000568, -32.23124999877096997, 98.26794919243111792 ) ) ;
#1550 = CARTESIAN_POINT ( 'NONE',  ( -81.02178482187500208, -32.20312499938548711, -102.3871387122750889 ) ) ;
#1551 = CARTESIAN_POINT ( 'NONE',  ( 82.40000000000001990, -33.93750000000000711, 97.00000000000000000 ) ) ;
#1552 = CARTESIAN_POINT ( 'NONE',  ( -80.90000000000000568, -32.34374999877096712, -102.5980762113533018 ) ) ;
#1553 = CARTESIAN_POINT ( 'NONE',  ( 232.5999999999999375, -32.84062499938548285, 103.1828516163667899 ) ) ;
#1554 = CARTESIAN_POINT ( 'NONE',  ( -79.39999999999999147, -31.48518749875868394, 98.26794919243110371 ) ) ;
#1555 = CARTESIAN_POINT ( 'NONE',  ( -83.77821517812500929, -32.87812499938548427, 102.3871387122750889 ) ) ;
#1556 = CARTESIAN_POINT ( 'NONE',  ( -82.40000000000000568, -31.68750000000000711, 102.9999999999999858 ) ) ;
#1557 = CARTESIAN_POINT ( 'NONE',  ( 85.15643035625001289, -32.39062499938548711, 99.99999999999998579 ) ) ;
#1558 = CARTESIAN_POINT ( 'NONE',  ( 244.7999999999999545, -29.80000000000000426, -100.0000000000000000 ) ) ;
#1559 = DIRECTION ( 'NONE',  ( -0.000000000000000000, -1.000000000000000000, -0.000000000000000000 ) ) ;
#1560 = CARTESIAN_POINT ( 'NONE',  ( 79.39999999999999147, -34.63124999877096855, -98.26794919243110371 ) ) ;
#1561 = CARTESIAN_POINT ( 'NONE',  ( 235.5999999999999943, -34.31249999999999289, 101.7320508075688537 ) ) ;
#1562 = ORIENTED_EDGE ( 'NONE', *, *, #6040, .T. ) ;
#1563 = CARTESIAN_POINT ( 'NONE',  ( 235.3564303562499447, -34.11562499938548143, -48.40857419181671162 ) ) ;
#1564 = CARTESIAN_POINT ( 'NONE',  ( 0.000000000000000000, 0.000000000000000000, 0.000000000000000000 ) ) ;
#1565 = CARTESIAN_POINT ( 'NONE',  ( 229.5999999999999375, -34.85624999877096286, 101.7320508075688679 ) ) ;
#1566 = CARTESIAN_POINT ( 'NONE',  ( 235.5999999999999375, -33.31874999877096144, -50.00000000000011369 ) ) ;
#1567 = CARTESIAN_POINT ( 'NONE',  ( -81.02178482187500208, -34.49062499938548854, 102.3871387122750889 ) ) ;
#1568 = ORIENTED_EDGE ( 'NONE', *, *, #568, .T. ) ;
#1569 = ORIENTED_EDGE ( 'NONE', *, *, #6263, .T. ) ;
#1570 = CARTESIAN_POINT ( 'NONE',  ( -81.59615242270662350, -34.36740381056766580, -96.99999999999998579 ) ) ;
#1571 = CARTESIAN_POINT ( 'NONE',  ( -82.40000000000000568, -34.10624999877096997, 96.99999999999998579 ) ) ;
#1572 = CARTESIAN_POINT ( 'NONE',  ( -82.39999999999999147, -33.48750000000000426, -97.00000000000000000 ) ) ;
#1573 = EDGE_LOOP ( 'NONE', ( #4390, #11414, #129, #16411 ) ) ;
#1574 = CARTESIAN_POINT ( 'NONE',  ( -99.99999999999998579, -35.00000000000000000, -150.0000000000000000 ) ) ;
#1575 = FACE_BOUND ( 'NONE', #12964, .T. ) ;
#1576 = CARTESIAN_POINT ( 'NONE',  ( -85.15643035624999868, -32.91562499938549280, 101.5914258081833879 ) ) ;
#1577 = CARTESIAN_POINT ( 'NONE',  ( -79.39999999999999147, -34.68750000000000000, 98.26794919243110371 ) ) ;
#1578 = CARTESIAN_POINT ( 'NONE',  ( -79.39999999999999147, -32.41874999877096997, 99.99999999999998579 ) ) ;
#1579 = CARTESIAN_POINT ( 'NONE',  ( 0.000000000000000000, -3.031088913245533867, -1.750000000000002220 ) ) ;
#1580 = DIRECTION ( 'NONE',  ( 1.000000000000000000, 0.000000000000000000, 0.000000000000000000 ) ) ;
#1581 = DIRECTION ( 'NONE',  ( 0.000000000000000000, 0.000000000000000000, -1.000000000000000000 ) ) ;
#1582 = CARTESIAN_POINT ( 'NONE',  ( -83.20384757729337366, -34.35134618820330843, -97.00000000000000000 ) ) ;
#1583 = VERTEX_POINT ( 'NONE', #6296 ) ;
#1584 = CARTESIAN_POINT ( 'NONE',  ( -81.02178482187500208, -32.69062499938548427, -97.61286128772489690 ) ) ;
#1585 = CARTESIAN_POINT ( 'NONE',  ( 105.1999999999999744, -34.51168759575592304, 150.0000000000000000 ) ) ;
#1586 = B_SPLINE_CURVE_WITH_KNOTS ( 'NONE', 3,
 ( #5604, #14854, #17510, #14461, #14556 ),
 .UNSPECIFIED., .F., .F.,
 ( 4, 1, 4 ),
 ( 0.000000000000000000, 0.002309401076758505356, 0.004618802153517010713 ),
 .UNSPECIFIED. ) ;
#1587 = CARTESIAN_POINT ( 'NONE',  ( 235.5999999999999943, -33.86249999999999716, 101.7320508075688537 ) ) ;
#1588 = DIRECTION ( 'NONE',  ( -4.625929269271485791E-17, -1.000000000000000000, 0.000000000000000000 ) ) ;
#1589 = CARTESIAN_POINT ( 'NONE',  ( -82.39999999999999147, -31.15312499938548640, 96.81714838363319586 ) ) ;
#1590 = CARTESIAN_POINT ( 'NONE',  ( 230.2961164517930968, -35.00002705695767702, -51.92148140967023551 ) ) ;
#1591 = CARTESIAN_POINT ( 'NONE',  ( 229.8435696437499303, -31.94062499938547717, -50.00000000000011369 ) ) ;
#1592 = EDGE_CURVE ( 'NONE', #867, #14213, #19275, .T. ) ;
#1593 = ADVANCED_FACE ( 'NONE', ( #19245 ), #7034, .T. ) ;
#1594 = VERTEX_POINT ( 'NONE', #9 ) ;
#1595 = ORIENTED_EDGE ( 'NONE', *, *, #7912, .T. ) ;
#1596 = CARTESIAN_POINT ( 'NONE',  ( 99.99999999999994316, -32.00000000000000000, 150.0000000000000000 ) ) ;
#1597 = CARTESIAN_POINT ( 'NONE',  ( -85.40000000000000568, -30.86250000000000071, 101.7320508075688679 ) ) ;
#1598 = CARTESIAN_POINT ( 'NONE',  ( -83.90000000000000568, -31.21874999877097068, 102.5980762113533018 ) ) ;
#1599 = CARTESIAN_POINT ( 'NONE',  ( 79.39999999999999147, -32.06250000000000000, 98.26794919243113213 ) ) ;
#1600 = DIRECTION ( 'NONE',  ( 5.836151346627967635E-31, -2.699762333426451414E-47, -1.000000000000000000 ) ) ;
#1601 = CARTESIAN_POINT ( 'NONE',  ( 232.5999999999999375, -32.72812499938547859, 103.1828516163667899 ) ) ;
#1602 = CARTESIAN_POINT ( 'NONE',  ( 235.3564303562499447, -33.06562499938547717, -50.00000000000011369 ) ) ;
#1603 = CARTESIAN_POINT ( 'NONE',  ( 82.39999999999999147, -33.48750000000000426, -103.0000000000000000 ) ) ;
#1604 = EDGE_CURVE ( 'NONE', #5913, #4731, #14539, .T. ) ;
#1605 = CARTESIAN_POINT ( 'NONE',  ( 79.64356964374999848, -32.16562499938548569, -99.99999999999998579 ) ) ;
#1606 = ORIENTED_EDGE ( 'NONE', *, *, #1728, .F. ) ;
#1607 = CARTESIAN_POINT ( 'NONE',  ( 232.5999999999999375, -31.23749999999999361, -46.53589838486234953 ) ) ;
#1608 = EDGE_CURVE ( 'NONE', #14362, #14185, #5674, .T. ) ;
#1609 = CYLINDRICAL_SURFACE ( 'NONE', #8497, 3.000000000000002665 ) ;
#1610 = CARTESIAN_POINT ( 'NONE',  ( 81.02178482187500208, -32.09062499938548285, -97.61286128772489690 ) ) ;
#1611 = DIRECTION ( 'NONE',  ( 1.000000000000000000, 0.000000000000000000, 0.000000000000000000 ) ) ;
#1612 = CARTESIAN_POINT ( 'NONE',  ( -83.32052461991715120, -34.98323688327303671, 97.06736352196708140 ) ) ;
#1613 = CARTESIAN_POINT ( 'NONE',  ( 235.3564303562499447, -30.44062499938548072, -51.59142580818350865 ) ) ;
#1614 = CARTESIAN_POINT ( 'NONE',  ( -79.39999999999999147, -31.53750000000000497, 98.26794919243110371 ) ) ;
#1615 = ORIENTED_EDGE ( 'NONE', *, *, #11751, .T. ) ;
#1616 = DIRECTION ( 'NONE',  ( 1.000000000000000000, -0.000000000000000000, -2.407412430484046130E-31 ) ) ;
#1617 = CARTESIAN_POINT ( 'NONE',  ( -81.59615242270662350, -34.36740381056766580, 102.9999999999999858 ) ) ;
#1618 = CARTESIAN_POINT ( 'NONE',  ( 83.20395887649176814, -35.00000000000001421, 97.36341917746361219 ) ) ;
#1619 = CARTESIAN_POINT ( 'NONE',  ( -85.40000000000000568, -31.83356250001229881, 98.26794919243111792 ) ) ;
#1620 = CARTESIAN_POINT ( 'NONE',  ( -83.90000000000000568, -33.07500000000000284, -97.40192378864668399 ) ) ;
#1621 = CARTESIAN_POINT ( 'NONE',  ( 99.99999999999997158, -5.200000000000008171, -150.0000000000000000 ) ) ;
#1622 = CARTESIAN_POINT ( 'NONE',  ( 79.64356964375001269, -32.31562499938548427, 98.40857419181659793 ) ) ;
#1623 = CARTESIAN_POINT ( 'NONE',  ( -82.39999999999999147, -32.58750000000000568, 102.9999999999999858 ) ) ;
#1624 = CARTESIAN_POINT ( 'NONE',  ( 229.5999999999999375, -33.11249999999999716, -48.26794919243123161 ) ) ;
#1625 = DIRECTION ( 'NONE',  ( 0.000000000000000000, 0.000000000000000000, -1.000000000000000000 ) ) ;
#1626 = CARTESIAN_POINT ( 'NONE',  ( -82.39999999999999147, -31.26562499938549067, -103.1828516163667899 ) ) ;
#1627 = ORIENTED_EDGE ( 'NONE', *, *, #11751, .F. ) ;
#1628 = CARTESIAN_POINT ( 'NONE',  ( 81.02178482187500208, -30.85312499938548569, 102.3871387122750889 ) ) ;
#1629 = CARTESIAN_POINT ( 'NONE',  ( 82.40000000000000568, -34.55624999877097281, 102.9999999999999858 ) ) ;
#1630 = AXIS2_PLACEMENT_3D ( 'NONE', #8981, #4593, #2930 ) ;
#1631 = FACE_OUTER_BOUND ( 'NONE', #8929, .T. ) ;
#1632 = AXIS2_PLACEMENT_3D ( 'NONE', #9289, #13587, #3137 ) ;
#1633 = CARTESIAN_POINT ( 'NONE',  ( -79.64356964374999848, -31.82812499938548356, 99.99999999999998579 ) ) ;
#1634 = FACE_OUTER_BOUND ( 'NONE', #9231, .T. ) ;
#1635 = ORIENTED_EDGE ( 'NONE', *, *, #12151, .F. ) ;
#1636 = CARTESIAN_POINT ( 'NONE',  ( -79.39999999999999147, -30.26249999999999929, -98.26794919243113213 ) ) ;
#1637 = CARTESIAN_POINT ( 'NONE',  ( 3.948111298835276894, -0.6968132764964359849, -3.500000000000154987 ) ) ;
#1638 = CARTESIAN_POINT ( 'NONE',  ( 82.40000000000000568, -34.78124999877096712, -102.9999999999999858 ) ) ;
#1639 = EDGE_CURVE ( 'NONE', #531, #13951, #18644, .T. ) ;
#1640 = CARTESIAN_POINT ( 'NONE',  ( -81.02178482187500208, -34.15312499938548285, -97.61286128772489690 ) ) ;
#1641 = CARTESIAN_POINT ( 'NONE',  ( 232.5999999999999375, -29.99999999999999645, -47.00000000000010658 ) ) ;
#1642 = CARTESIAN_POINT ( 'NONE',  ( 231.2217848218749339, -31.52812499938548285, 102.3871387122750889 ) ) ;
#1643 = CARTESIAN_POINT ( 'NONE',  ( -83.90000000000000568, -33.02268749875867826, 102.5980762113533018 ) ) ;
#1644 = CARTESIAN_POINT ( 'NONE',  ( -79.64356964374999848, -33.17812499938548854, 99.99999999999998579 ) ) ;
#1645 = CARTESIAN_POINT ( 'NONE',  ( -82.39999999999999147, -34.30312499938548143, -103.1828516163667899 ) ) ;
#1646 = CARTESIAN_POINT ( 'NONE',  ( 81.02178482187500208, -32.54062499938548569, 102.3871387122750889 ) ) ;
#1647 = DIRECTION ( 'NONE',  ( -0.000000000000000000, -1.000000000000000000, -0.000000000000000000 ) ) ;
#1648 = VECTOR ( 'NONE', #8322, 1000.000000000000000 ) ;
#1649 = VECTOR ( 'NONE', #3154, 1000.000000000000000 ) ;
#1650 = CARTESIAN_POINT ( 'NONE',  ( 83.90000000000000568, -32.62500000000000000, -102.5980762113533018 ) ) ;
#1651 = CARTESIAN_POINT ( 'NONE',  ( 85.40000000000000568, -34.03124999877096712, -98.26794919243111792 ) ) ;
#1652 = CARTESIAN_POINT ( 'NONE',  ( 235.5999999999999943, -32.43749999999999289, 98.26794919243110371 ) ) ;
#1653 = ORIENTED_EDGE ( 'NONE', *, *, #6826, .T. ) ;
#1654 = CARTESIAN_POINT ( 'NONE',  ( 233.9782151781249411, -33.25312499938547717, -47.61286128772501769 ) ) ;
#1655 = CARTESIAN_POINT ( 'NONE',  ( 0.000000000000000000, 0.000000000000000000, 0.000000000000000000 ) ) ;
#1656 = CARTESIAN_POINT ( 'NONE',  ( 231.2217848218749339, -31.22812499938547859, 97.61286128772489690 ) ) ;
#1657 = CARTESIAN_POINT ( 'NONE',  ( 232.5999999999999375, -32.98124999877096286, -46.53589838486234953 ) ) ;
#1658 = CARTESIAN_POINT ( 'NONE',  ( -85.15643035625001289, -33.29062499938547859, 99.99999999999998579 ) ) ;
#1659 = EDGE_LOOP ( 'NONE', ( #11246, #808 ) ) ;
#1660 = ORIENTED_EDGE ( 'NONE', *, *, #11468, .T. ) ;
#1661 = CARTESIAN_POINT ( 'NONE',  ( 4.104070371397485317, 2.023683613428365113, -3.505122836902508698 ) ) ;
#1662 = VECTOR ( 'NONE', #515, 1000.000000000000000 ) ;
#1663 = CARTESIAN_POINT ( 'NONE',  ( -85.40000000000000568, -34.95000000000000284, 99.99999999999998579 ) ) ;
#1664 = CARTESIAN_POINT ( 'NONE',  ( -83.20384757729337366, -33.50759618943233420, -97.00000000000000000 ) ) ;
#1665 = VERTEX_POINT ( 'NONE', #14443 ) ;
#1666 = CARTESIAN_POINT ( 'NONE',  ( -4.000000000000000000, 0.7924765000094600165, -0.05906175389889745803 ) ) ;
#1667 = DIRECTION ( 'NONE',  ( -0.000000000000000000, 3.469446951953616161E-16, -1.000000000000000000 ) ) ;
#1668 = CARTESIAN_POINT ( 'NONE',  ( -83.77821517812500929, -34.22812499938549280, 102.3871387122750889 ) ) ;
#1669 = CARTESIAN_POINT ( 'NONE',  ( -85.40000000000000568, -34.05000000000000426, 99.99999999999998579 ) ) ;
#1670 = CARTESIAN_POINT ( 'NONE',  ( -83.90000000000000568, -32.71874999877096712, 97.40192378864668399 ) ) ;
#1671 = CARTESIAN_POINT ( 'NONE',  ( -82.40000000000000568, -30.00000000000000355, 99.99999999999998579 ) ) ;
#1672 = FACE_BOUND ( 'NONE', #5012, .T. ) ;
#1673 = CARTESIAN_POINT ( 'NONE',  ( 82.40000000000000568, -30.00000000000000355, 96.99999999999998579 ) ) ;
#1674 = CARTESIAN_POINT ( 'NONE',  ( -79.39999999999999147, -34.66874999877096997, -99.99999999999998579 ) ) ;
#1675 = CARTESIAN_POINT ( 'NONE',  ( 232.5999999999999375, -32.05312499938548143, 96.81714838363319586 ) ) ;
#1676 = ORIENTED_EDGE ( 'NONE', *, *, #496, .T. ) ;
#1677 = ADVANCED_FACE ( 'NONE', ( #16221, #14639 ), #1076, .F. ) ;
#1678 = CARTESIAN_POINT ( 'NONE',  ( -79.64356964374999848, -34.41562499938548569, -99.99999999999998579 ) ) ;
#1679 = CARTESIAN_POINT ( 'NONE',  ( 25.60000000000000142, 2.516649172247811061E-16, -2.055000000000000160 ) ) ;
#1680 = DIRECTION ( 'NONE',  ( -1.000000000000000000, 0.000000000000000000, 0.000000000000000000 ) ) ;
#1681 = PLANE ( 'NONE',  #8961 ) ;
#1682 = CARTESIAN_POINT ( 'NONE',  ( 83.90000000000000568, -33.22500000000000142, -97.40192378864668399 ) ) ;
#1683 = CARTESIAN_POINT ( 'NONE',  ( 231.2217848218749339, -34.11562499938548143, -47.61286128772501769 ) ) ;
#1684 = ORIENTED_EDGE ( 'NONE', *, *, #2088, .T. ) ;
#1685 = EDGE_LOOP ( 'NONE', ( #4885, #3401, #822, #4248, #3393, #10422, #9731 ) ) ;
#1686 = CARTESIAN_POINT ( 'NONE',  ( -2.059999999999998721, 2.522772406243545965E-16, -0.3080913168122742518 ) ) ;
#1687 = CARTESIAN_POINT ( 'NONE',  ( -79.39999999999999147, -30.18750000000000355, 98.26794919243110371 ) ) ;
#1688 = CARTESIAN_POINT ( 'NONE',  ( -79.39999999999999147, -31.48124999877097352, 98.26794919243110371 ) ) ;
#1689 = CARTESIAN_POINT ( 'NONE',  ( 85.40000000000000568, -30.90000000000000213, 99.99999999999998579 ) ) ;
#1690 = CARTESIAN_POINT ( 'NONE',  ( -81.68701737470176738, -31.99999999999998579, -97.18802777794499548 ) ) ;
#1691 = CARTESIAN_POINT ( 'NONE',  ( 232.5999999999999375, -34.30312499938547433, 96.81714838363319586 ) ) ;
#1692 = CARTESIAN_POINT ( 'NONE',  ( 83.20384757729335945, -32.28615380933863577, 103.0000000000000000 ) ) ;
#1693 = CARTESIAN_POINT ( 'NONE',  ( 80.80006050676068696, -31.99999999999999289, -97.54622936385604248 ) ) ;
#1694 = CARTESIAN_POINT ( 'NONE',  ( 79.64356964374999848, -33.51562499938548711, -99.99999999999998579 ) ) ;
#1695 = EDGE_LOOP ( 'NONE', ( #1173, #10213, #9283, #2397 ) ) ;
#1696 = CARTESIAN_POINT ( 'NONE',  ( 235.5999999999999943, -32.88749999999998863, -51.73205080756900287 ) ) ;
#1697 = CARTESIAN_POINT ( 'NONE',  ( -82.39999999999999147, -34.52812499938548285, 103.1828516163667899 ) ) ;
#1698 = CARTESIAN_POINT ( 'NONE',  ( 81.02178482187500208, -33.14062499938548711, -102.3871387122750889 ) ) ;
#1699 = DIRECTION ( 'NONE',  ( 0.000000000000000000, 0.000000000000000000, 1.000000000000000000 ) ) ;
#1700 = CARTESIAN_POINT ( 'NONE',  ( -79.39999999999999147, -34.66874999877096997, 99.99999999999998579 ) ) ;
#1701 = CARTESIAN_POINT ( 'NONE',  ( 232.5999999999999375, -32.84062499938548285, -46.81714838363331666 ) ) ;
#1702 = CARTESIAN_POINT ( 'NONE',  ( -79.39999999999999147, -30.26249999999999929, 101.7320508075688537 ) ) ;
#1703 = ORIENTED_EDGE ( 'NONE', *, *, #1293, .F. ) ;
#1704 = CARTESIAN_POINT ( 'NONE',  ( -84.94178044275902550, -34.99917348188823496, 101.6311593377337203 ) ) ;
#1705 = CARTESIAN_POINT ( 'NONE',  ( 229.8435696437499587, -34.22812499938547859, 98.40857419181659793 ) ) ;
#1706 = CARTESIAN_POINT ( 'NONE',  ( 8.673617379884035472E-16, 4.618802153517012954, -5.000000000000000000 ) ) ;
#1707 = CARTESIAN_POINT ( 'NONE',  ( -80.90000000000000568, -33.29606250001229739, 97.40192378864668399 ) ) ;
#1708 = CARTESIAN_POINT ( 'NONE',  ( 1.144235203016666258, 3.958177651039090250, -0.09382832055445661235 ) ) ;
#1709 = CARTESIAN_POINT ( 'NONE',  ( -79.64356964374999848, -31.82812499938548356, 99.99999999999998579 ) ) ;
#1710 = CARTESIAN_POINT ( 'NONE',  ( 231.5655627039825504, -35.00000000000000000, 102.5775038898417080 ) ) ;
#1711 = CARTESIAN_POINT ( 'NONE',  ( 85.15643035624999868, -34.26562499938548711, 98.40857419181659793 ) ) ;
#1712 = EDGE_CURVE ( 'NONE', #12416, #7197, #10347, .T. ) ;
#1713 = CARTESIAN_POINT ( 'NONE',  ( 79.64356964375001269, -30.51562499938548711, -101.5914258081833879 ) ) ;
#1714 = CARTESIAN_POINT ( 'NONE',  ( 232.5999999999999375, -31.60312499938548214, -53.18285161636690361 ) ) ;
#1715 = CARTESIAN_POINT ( 'NONE',  ( 82.39999999999999147, -35.09062499938548285, -103.1828516163667899 ) ) ;
#1716 = CARTESIAN_POINT ( 'NONE',  ( -85.15643035624999868, -34.26562499938548711, -98.40857419181659793 ) ) ;
#1717 = VERTEX_POINT ( 'NONE', #8874 ) ;
#1718 = CARTESIAN_POINT ( 'NONE',  ( 79.64356964375001269, -30.96562499938548640, 98.40857419181659793 ) ) ;
#1719 = DIRECTION ( 'NONE',  ( 7.222237291452147586E-32, -1.214306433183764966E-16, 1.000000000000000000 ) ) ;
#1720 = CARTESIAN_POINT ( 'NONE',  ( -85.15643035624999868, -31.11562499938548854, 101.5914258081833879 ) ) ;
#1721 = CARTESIAN_POINT ( 'NONE',  ( -1.828356344711647319, -3.563200125723192002, -1.076197711133951296E-14 ) ) ;
#1722 = ORIENTED_EDGE ( 'NONE', *, *, #10017, .T. ) ;
#1723 = EDGE_CURVE ( 'NONE', #16053, #18412, #14010, .T. ) ;
#1724 = CARTESIAN_POINT ( 'NONE',  ( -83.90000000000000568, -31.87500000000000000, -102.5980762113533018 ) ) ;
#1725 = EDGE_CURVE ( 'NONE', #4443, #17789, #10375, .T. ) ;
#1726 = CARTESIAN_POINT ( 'NONE',  ( 82.40000000000001990, -33.88124999877096855, 97.00000000000000000 ) ) ;
#1727 = CARTESIAN_POINT ( 'NONE',  ( -82.39999999999999147, -34.19062499938548427, -96.81714838363319586 ) ) ;
#1728 = EDGE_CURVE ( 'NONE', #18944, #3617, #17178, .T. ) ;
#1729 = FACE_OUTER_BOUND ( 'NONE', #16285, .T. ) ;
#1730 = CARTESIAN_POINT ( 'NONE',  ( 235.3564303562499447, -34.52812499938547575, 99.99999999999998579 ) ) ;
#1731 = CARTESIAN_POINT ( 'NONE',  ( -85.40000000000000568, -31.33518749875867471, 98.26794919243111792 ) ) ;
#1732 = ORIENTED_EDGE ( 'NONE', *, *, #12259, .T. ) ;
#1733 = CARTESIAN_POINT ( 'NONE',  ( -83.77821517812500929, -33.47812499938548569, 97.61286128772489690 ) ) ;
#1734 = CARTESIAN_POINT ( 'NONE',  ( -82.05869624310419397, -34.96883842999724124, -97.01420019955241969 ) ) ;
#1735 = CARTESIAN_POINT ( 'NONE',  ( 83.77821517812500929, -32.31562499938548427, 97.61286128772489690 ) ) ;
#1736 = CARTESIAN_POINT ( 'NONE',  ( 83.90000000000000568, -34.36874999877097281, -102.5980762113533018 ) ) ;
#1737 = CIRCLE ( 'NONE', #11087, 7.000000000000006217 ) ;
#1738 = CARTESIAN_POINT ( 'NONE',  ( 82.39999999999999147, -32.58750000000000568, -102.9999999999999858 ) ) ;
#1739 = CARTESIAN_POINT ( 'NONE',  ( 85.40000000000000568, -33.13124999877096855, -98.26794919243111792 ) ) ;
#1740 = CARTESIAN_POINT ( 'NONE',  ( 229.5999999999999375, -34.46249999999999147, 101.7320508075688679 ) ) ;
#1741 = ORIENTED_EDGE ( 'NONE', *, *, #7576, .F. ) ;
#1742 = CARTESIAN_POINT ( 'NONE',  ( 232.5999999999999943, -32.84062499938548285, -46.81714838363331666 ) ) ;
#1743 = DIRECTION ( 'NONE',  ( 4.814824860968092260E-31, -1.336382355046098552E-47, 1.000000000000000000 ) ) ;
#1744 = ADVANCED_FACE ( 'NONE', ( #9451 ), #5922, .F. ) ;
#1745 = CARTESIAN_POINT ( 'NONE',  ( 229.5999999999999375, -34.93124999877095860, 98.26794919243111792 ) ) ;
#1746 = CARTESIAN_POINT ( 'NONE',  ( 229.5999999999999375, -35.34374999877096002, -50.00000000000011369 ) ) ;
#1747 = CARTESIAN_POINT ( 'NONE',  ( 100.0000000000000000, 10.19999999999999218, -140.0000000000000000 ) ) ;
#1748 = ORIENTED_EDGE ( 'NONE', *, *, #5307, .T. ) ;
#1749 = ORIENTED_EDGE ( 'NONE', *, *, #19047, .T. ) ;
#1750 = CARTESIAN_POINT ( 'NONE',  ( 4.093692494532770176, 2.021783646005773427, -3.501831996793853818 ) ) ;
#1751 = VECTOR ( 'NONE', #13002, 1000.000000000000000 ) ;
#1752 = FACE_OUTER_BOUND ( 'NONE', #19008, .T. ) ;
#1753 = DIRECTION ( 'NONE',  ( -1.000000000000000000, -0.000000000000000000, -0.000000000000000000 ) ) ;
#1754 = ORIENTED_EDGE ( 'NONE', *, *, #13096, .T. ) ;
#1755 = DIRECTION ( 'NONE',  ( -0.000000000000000000, -1.000000000000000000, -0.000000000000000000 ) ) ;
#1756 = FACE_OUTER_BOUND ( 'NONE', #9533, .T. ) ;
#1757 = CARTESIAN_POINT ( 'NONE',  ( -81.02178482187500208, -33.70312499938548711, 102.3871387122750889 ) ) ;
#1758 = CARTESIAN_POINT ( 'NONE',  ( -79.39999999999999147, -34.31250000000000000, 101.7320508075688537 ) ) ;
#1759 = EDGE_CURVE ( 'NONE', #4731, #17788, #9431, .T. ) ;
#1760 = CARTESIAN_POINT ( 'NONE',  ( -80.90000000000000568, -31.44374999877096855, 97.40192378864668399 ) ) ;
#1761 = PLANE ( 'NONE',  #421 ) ;
#1762 = CARTESIAN_POINT ( 'NONE',  ( 82.40000000000000568, -30.00000000000000355, 96.99999999999998579 ) ) ;
#1763 = CARTESIAN_POINT ( 'NONE',  ( 249.9999999999999716, -35.00000000000000000, -100.0000000000000000 ) ) ;
#1764 = CARTESIAN_POINT ( 'NONE',  ( 5.599999999999999645, 0.000000000000000000, 2.500000000000000444 ) ) ;
#1765 = LINE ( 'NONE', #220, #18039 ) ;
#1766 = CARTESIAN_POINT ( 'NONE',  ( 232.5999999999999375, -32.27812499938547575, 103.1828516163667899 ) ) ;
#1767 = ORIENTED_EDGE ( 'NONE', *, *, #12376, .T. ) ;
#1768 = CARTESIAN_POINT ( 'NONE',  ( -82.39999999999999147, -32.95312499938548711, -103.1828516163667899 ) ) ;
#1769 = DIRECTION ( 'NONE',  ( -0.000000000000000000, 1.000000000000000000, 0.000000000000000000 ) ) ;
#1770 = CARTESIAN_POINT ( 'NONE',  ( 0.000000000000000000, 0.000000000000000000, -4.974599999999998801 ) ) ;
#1771 = CARTESIAN_POINT ( 'NONE',  ( 231.7961524227065695, -34.35134618820329422, 103.0000000000000000 ) ) ;
#1772 = CARTESIAN_POINT ( 'NONE',  ( 4.000000000000000000, 2.309401076758515803, -0.4999999999999995559 ) ) ;
#1773 = CARTESIAN_POINT ( 'NONE',  ( 233.9782151781249411, -34.49062499938548143, -47.61286128772501769 ) ) ;
#1774 = CARTESIAN_POINT ( 'NONE',  ( 229.8435696437499303, -32.50312499938547717, 99.99999999999998579 ) ) ;
#1775 = EDGE_LOOP ( 'NONE', ( #3436, #14144, #6656, #3600 ) ) ;
#1776 = VERTEX_POINT ( 'NONE', #11380 ) ;
#1777 = CARTESIAN_POINT ( 'NONE',  ( 82.39999999999999147, -33.20624999877097849, -97.00000000000000000 ) ) ;
#1778 = CARTESIAN_POINT ( 'NONE',  ( 79.39999999999999147, -30.22500000000000142, -99.99999999999998579 ) ) ;
#1779 = CARTESIAN_POINT ( 'NONE',  ( -85.40000000000000568, -32.23124999877096997, 98.26794919243111792 ) ) ;
#1780 = CARTESIAN_POINT ( 'NONE',  ( 83.90000000000000568, -32.32500000000000284, 102.5980762113533018 ) ) ;
#1781 = DIRECTION ( 'NONE',  ( -0.000000000000000000, -0.000000000000000000, -1.000000000000000000 ) ) ;
#1782 = CARTESIAN_POINT ( 'NONE',  ( 233.9782151781249411, -34.49062499938548143, 102.3871387122750889 ) ) ;
#1783 = CARTESIAN_POINT ( 'NONE',  ( 82.39999999999999147, -32.84062499938548996, -103.1828516163667899 ) ) ;
#1784 = VECTOR ( 'NONE', #18195, 1000.000000000000000 ) ;
#1785 = CARTESIAN_POINT ( 'NONE',  ( 4.000000000000000000, -2.309401076758516691, -0.4999999999999995559 ) ) ;
#1786 = CARTESIAN_POINT ( 'NONE',  ( 79.64356964375001269, -32.65312499938548285, -101.5914258081833879 ) ) ;
#1787 = ORIENTED_EDGE ( 'NONE', *, *, #2182, .F. ) ;
#1788 = CARTESIAN_POINT ( 'NONE',  ( 231.0999999999999375, -33.67499999999999716, -52.59807621135342970 ) ) ;
#1789 = CARTESIAN_POINT ( 'NONE',  ( -82.40000000000001990, -34.16250000000000853, 97.00000000000000000 ) ) ;
#1790 = CARTESIAN_POINT ( 'NONE',  ( 85.15643035624999868, -32.80312499938548854, -101.5914258081833879 ) ) ;
#1791 = AXIS2_PLACEMENT_3D ( 'NONE', #13750, #7986, #6342 ) ;
#1792 = DIRECTION ( 'NONE',  ( 0.000000000000000000, 0.000000000000000000, -1.000000000000000000 ) ) ;
#1793 = CARTESIAN_POINT ( 'NONE',  ( -81.02178482187500208, -32.20312499938548711, 97.61286128772489690 ) ) ;
#1794 = CARTESIAN_POINT ( 'NONE',  ( 232.5999999999999375, -32.39062499938548001, -46.81714838363331666 ) ) ;
#1795 = CARTESIAN_POINT ( 'NONE',  ( -83.77821517812500929, -35.01562499938548711, 102.3871387122750889 ) ) ;
#1796 = EDGE_LOOP ( 'NONE', ( #14638, #7352, #14844, #15299 ) ) ;
#1797 = CARTESIAN_POINT ( 'NONE',  ( -79.39923258946704721, -35.00058613678730524, 99.84651357762385260 ) ) ;
#1798 = CARTESIAN_POINT ( 'NONE',  ( -80.90000000000000568, -31.14374999877097139, 102.5980762113533018 ) ) ;
#1799 = CARTESIAN_POINT ( 'NONE',  ( 83.77821517812500929, -30.66562499938548569, 102.3871387122750889 ) ) ;
#1800 = AXIS2_PLACEMENT_3D ( 'NONE', #15147, #16426, #4607 ) ;
#1801 = VECTOR ( 'NONE', #2887, 1000.000000000000000 ) ;
#1802 = CARTESIAN_POINT ( 'NONE',  ( 84.97866794691725545, -31.99999999999998579, -99.01001922939877886 ) ) ;
#1803 = CARTESIAN_POINT ( 'NONE',  ( -85.15643035625001289, -30.66562499938548569, 101.5914258081833879 ) ) ;
#1804 = CARTESIAN_POINT ( 'NONE',  ( -82.39999999999999147, -32.58750000000000568, 102.9999999999999858 ) ) ;
#1805 = CARTESIAN_POINT ( 'NONE',  ( 84.51154815724953551, -35.25364861271051353, 101.7717992799616553 ) ) ;
#1806 = CARTESIAN_POINT ( 'NONE',  ( 83.77821517812500929, -31.07812499938548711, -102.3871387122750889 ) ) ;
#1807 = AXIS2_PLACEMENT_3D ( 'NONE', #10995, #6415, #6609 ) ;
#1808 = DIRECTION ( 'NONE',  ( 0.000000000000000000, 0.000000000000000000, -1.000000000000000000 ) ) ;
#1809 = CARTESIAN_POINT ( 'NONE',  ( -84.97866794691721282, -32.00000000000001421, -100.9899807706014485 ) ) ;
#1810 = CARTESIAN_POINT ( 'NONE',  ( -83.77821517812500929, -32.57812499938548711, -102.3871387122750889 ) ) ;
#1811 = ORIENTED_EDGE ( 'NONE', *, *, #6489, .F. ) ;
#1812 = CARTESIAN_POINT ( 'NONE',  ( 80.90000000000000568, -35.19374999877096855, 97.40192378864668399 ) ) ;
#1813 = CARTESIAN_POINT ( 'NONE',  ( -83.90000000000000568, -33.01874999877097139, 102.5980762113533018 ) ) ;
#1814 = VECTOR ( 'NONE', #818, 1000.000000000000000 ) ;
#1815 = ADVANCED_FACE ( 'NONE', ( #16069 ), #2580, .T. ) ;
#1816 = DIRECTION ( 'NONE',  ( 0.000000000000000000, 0.000000000000000000, -1.000000000000000000 ) ) ;
#1817 = CARTESIAN_POINT ( 'NONE',  ( -81.02178482187500208, -32.80312499938548854, 102.3871387122750889 ) ) ;
#1818 = CARTESIAN_POINT ( 'NONE',  ( 5.599999999999999645, -2.020725942163688060, 3.500000000000000444 ) ) ;
#1819 = ORIENTED_EDGE ( 'NONE', *, *, #7074, .F. ) ;
#1820 = CARTESIAN_POINT ( 'NONE',  ( -83.90000000000000568, -32.17500000000000426, -97.40192378864668399 ) ) ;
#1821 = ADVANCED_FACE ( 'NONE', ( #14592 ), #17561, .T. ) ;
#1822 = ADVANCED_FACE ( 'NONE', ( #7179 ), #13129, .F. ) ;
#1823 = CARTESIAN_POINT ( 'NONE',  ( 80.90000000000000568, -34.20000000000000284, -97.40192378864668399 ) ) ;
#1824 = CARTESIAN_POINT ( 'NONE',  ( 81.59615242270665192, -33.86115380933864571, 97.00000000000000000 ) ) ;
#1825 = CARTESIAN_POINT ( 'NONE',  ( -85.15643035624999868, -34.79062499938548569, -101.5914258081833879 ) ) ;
#1826 = CARTESIAN_POINT ( 'NONE',  ( 5.599999999999999645, -4.041451884327388555, 0.000000000000000000 ) ) ;
#1827 = CARTESIAN_POINT ( 'NONE',  ( 229.8435696437499871, -34.79062499938547859, 98.40857419181659793 ) ) ;
#1828 = CARTESIAN_POINT ( 'NONE',  ( -83.90000000000000568, -31.82268749875867542, 97.40192378864668399 ) ) ;
#1829 = ORIENTED_EDGE ( 'NONE', *, *, #5453, .T. ) ;
#1830 = CARTESIAN_POINT ( 'NONE',  ( 231.0999999999999375, -32.62499999999999289, 102.5980762113533018 ) ) ;
#1831 = CARTESIAN_POINT ( 'NONE',  ( 83.20384757729337366, -32.34240381056766722, 103.0000000000000000 ) ) ;
#1832 = CARTESIAN_POINT ( 'NONE',  ( 85.15643035625001289, -33.77812499938548285, 101.5914258081833879 ) ) ;
#1833 = CARTESIAN_POINT ( 'NONE',  ( 111.0000000000000000, 15.19999999999997620, -143.3166247903554336 ) ) ;
#1834 = DIRECTION ( 'NONE',  ( 0.000000000000000000, 0.000000000000000000, -1.000000000000000000 ) ) ;
#1835 = CARTESIAN_POINT ( 'NONE',  ( 80.90000000000000568, -34.14374999877097139, -97.40192378864668399 ) ) ;
#1836 = CYLINDRICAL_SURFACE ( 'NONE', #10218, 3.000000000000002665 ) ;
#1837 = ADVANCED_FACE ( 'NONE', ( #9921 ), #16171, .F. ) ;
#1838 = ORIENTED_EDGE ( 'NONE', *, *, #290, .F. ) ;
#1839 = CARTESIAN_POINT ( 'NONE',  ( 231.2217848218749339, -32.42812499938548143, -47.61286128772501769 ) ) ;
#1840 = CARTESIAN_POINT ( 'NONE',  ( 0.000000000000000000, 0.000000000000000000, 0.000000000000000000 ) ) ;
#1841 = CARTESIAN_POINT ( 'NONE',  ( 231.0999999999999375, -34.51874999877096428, 97.40192378864668399 ) ) ;
#1842 = EDGE_CURVE ( 'NONE', #5588, #19181, #14688, .T. ) ;
#1843 = CARTESIAN_POINT ( 'NONE',  ( 231.0999999999999375, -35.26874999877096428, -47.40192378864679768 ) ) ;
#1844 = APPLICATION_CONTEXT ( 'automotive_design' ) ;
#1845 = CARTESIAN_POINT ( 'NONE',  ( -85.15643035625001289, -35.09062499938548285, 99.99999999999998579 ) ) ;
#1846 = ORIENTED_EDGE ( 'NONE', *, *, #7551, .F. ) ;
#1847 = ORIENTED_EDGE ( 'NONE', *, *, #3268, .T. ) ;
#1848 = CARTESIAN_POINT ( 'NONE',  ( -79.64356964375001269, -30.40312499938548285, -98.40857419181659793 ) ) ;
#1849 = CARTESIAN_POINT ( 'NONE',  ( 96.99999999999997158, -5.200000000000003730, -150.0000000000000000 ) ) ;
#1850 = CARTESIAN_POINT ( 'NONE',  ( 4.071447262713890680, -4.041451884327388555, 0.000000000000000000 ) ) ;
#1851 = ORIENTED_EDGE ( 'NONE', *, *, #12808, .F. ) ;
#1852 = CARTESIAN_POINT ( 'NONE',  ( 84.44763168836732348, -32.00000000000002132, 98.15470523285560489 ) ) ;
#1853 = CYLINDRICAL_SURFACE ( 'NONE', #11735, 2.199999999999993516 ) ;
#1854 = LINE ( 'NONE', #16807, #16932 ) ;
#1855 = CARTESIAN_POINT ( 'NONE',  ( -83.90000000000000568, -33.97500000000000853, 102.5980762113533018 ) ) ;
#1856 = CARTESIAN_POINT ( 'NONE',  ( -79.39999999999999147, -34.66874999877096997, 99.99999999999998579 ) ) ;
#1857 = CARTESIAN_POINT ( 'NONE',  ( -81.59615242270662350, -30.52634618820330914, 97.00000000000000000 ) ) ;
#1858 = CARTESIAN_POINT ( 'NONE',  ( -79.39999999999999147, -30.67500000000000071, 99.99999999999998579 ) ) ;
#1859 = FILL_AREA_STYLE_COLOUR ( '', #13186 ) ;
#1860 = CARTESIAN_POINT ( 'NONE',  ( 4.086376042167607636, 4.082715877136865679, -0.07147133206918158954 ) ) ;
#1861 = CARTESIAN_POINT ( 'NONE',  ( 229.8435696437499871, -34.67812499938547433, 98.40857419181659793 ) ) ;
#1862 = CARTESIAN_POINT ( 'NONE',  ( 233.9782151781249411, -32.09062499938547575, 97.61286128772489690 ) ) ;
#1863 = ORIENTED_EDGE ( 'NONE', *, *, #14991, .T. ) ;
#1864 =( NAMED_UNIT ( * ) PLANE_ANGLE_UNIT ( ) SI_UNIT ( $, .RADIAN. ) );
#1865 = CARTESIAN_POINT ( 'NONE',  ( -81.02178482187500208, -33.14062499938548711, -97.61286128772489690 ) ) ;
#1866 = LINE ( 'NONE', #611, #2732 ) ;
#1867 = EDGE_LOOP ( 'NONE', ( #1943, #15394, #2168, #4100 ) ) ;
#1868 = ADVANCED_FACE ( 'NONE', ( #11479 ), #13038, .F. ) ;
#1869 = CARTESIAN_POINT ( 'NONE',  ( 4.211140560182196957, 2.431303136016536470, -3.745885042887433514 ) ) ;
#1870 = CYLINDRICAL_SURFACE ( 'NONE', #16156, 3.000000000000002665 ) ;
#1871 = CYLINDRICAL_SURFACE ( 'NONE', #4749, 3.000000000000002665 ) ;
#1872 = DIRECTION ( 'NONE',  ( -0.000000000000000000, -1.000000000000000000, -0.000000000000000000 ) ) ;
#1873 = ORIENTED_EDGE ( 'NONE', *, *, #18310, .F. ) ;
#1874 = EDGE_LOOP ( 'NONE', ( #6386, #6158, #12245, #13159 ) ) ;
#1875 = CARTESIAN_POINT ( 'NONE',  ( -99.99999999999998579, -29.80000000000000426, -150.0000000000000000 ) ) ;
#1876 = CARTESIAN_POINT ( 'NONE',  ( 82.39999999999999147, -31.23750000000000071, -103.4641016151377499 ) ) ;
#1877 = CARTESIAN_POINT ( 'NONE',  ( -83.90000000000000568, -34.36874999877097281, 102.5980762113533018 ) ) ;
#1878 = ADVANCED_FACE ( 'NONE', ( #10493 ), #15082, .F. ) ;
#1879 = DIRECTION ( 'NONE',  ( -1.000000000000000000, 0.000000000000000000, 0.000000000000000000 ) ) ;
#1880 = CARTESIAN_POINT ( 'NONE',  ( 235.3564303562499447, -33.55312499938548143, 101.5914258081833879 ) ) ;
#1881 = CARTESIAN_POINT ( 'NONE',  ( 79.64356964374998427, -32.24062499938548854, -98.40857419181659793 ) ) ;
#1882 = DIRECTION ( 'NONE',  ( 0.000000000000000000, 0.000000000000000000, -1.000000000000000000 ) ) ;
#1883 = CARTESIAN_POINT ( 'NONE',  ( 82.39999999999999147, -33.40312499938548285, -96.81714838363319586 ) ) ;
#1884 = VERTEX_POINT ( 'NONE', #13516 ) ;
#1885 = B_SPLINE_CURVE_WITH_KNOTS ( 'NONE', 3,
 ( #9094, #13401, #18103, #33, #17906, #4512, #10468, #16434, #3043, #9005, #134, #13495, #3431, #14073, #9288, #12224 ),
 .UNSPECIFIED., .F., .F.,
 ( 4, 2, 2, 2, 2, 2, 2, 4 ),
 ( 0.000000000000000000, 0.0005391024520904479393, 0.001078204904180895879, 0.002156409808361764869, 0.002695512260452209014, 0.003234614712542652724, 0.003773717164633096869, 0.004312819616723541014 ),
 .UNSPECIFIED. ) ;
#1886 = CARTESIAN_POINT ( 'NONE',  ( 234.0999999999999375, -31.49999999999999289, -52.59807621135342970 ) ) ;
#1887 = CARTESIAN_POINT ( 'NONE',  ( -85.40000000000000568, -34.91250000000000142, 101.7320508075688679 ) ) ;
#1888 = B_SPLINE_CURVE_WITH_KNOTS ( 'NONE', 3,
 ( #7594, #16391, #19134, #13259, #10247, #13363, #17669, #91, #5751, #19233, #2385, #11991, #5849, #16209, #11700, #17772, #4379, #4474 ),
 .UNSPECIFIED., .F., .F.,
 ( 4, 2, 2, 2, 2, 2, 2, 2, 4 ),
 ( 0.000000000000000000, 0.0007089252359966202559, 0.001417850471993240512, 0.002126775707989860768, 0.002835700943986481024, 0.003544626179983101279, 0.004253551415979721535, 0.004962476651976341357, 0.005671401887972962047 ),
 .UNSPECIFIED. ) ;
#1889 = CARTESIAN_POINT ( 'NONE',  ( -83.90000000000000568, -33.91874999877096997, 102.5980762113533018 ) ) ;
#1890 = CARTESIAN_POINT ( 'NONE',  ( 229.8435696437499303, -33.40312499938547575, 99.99999999999998579 ) ) ;
#1891 = CARTESIAN_POINT ( 'NONE',  ( -83.77821517812500929, -30.62812499938548783, 102.3871387122750889 ) ) ;
#1892 = CARTESIAN_POINT ( 'NONE',  ( 231.2217848218749339, -33.02812499938547575, -52.38713871227520968 ) ) ;
#1893 = CARTESIAN_POINT ( 'NONE',  ( -82.39999999999999147, -31.23750000000000071, 103.4641016151377499 ) ) ;
#1894 = VERTEX_POINT ( 'NONE', #2969 ) ;
#1895 = CARTESIAN_POINT ( 'NONE',  ( -83.35106844018336858, -35.00071516271440686, 102.8502752770200601 ) ) ;
#1896 = CARTESIAN_POINT ( 'NONE',  ( 235.3564303562499447, -34.41562499938547859, 99.99999999999998579 ) ) ;
#1897 = CARTESIAN_POINT ( 'NONE',  ( -81.59615242270662350, -32.56740381056766864, 103.0000000000000000 ) ) ;
#1898 = CARTESIAN_POINT ( 'NONE',  ( 229.8538686580537558, -31.99999999999998579, -50.29785994008192773 ) ) ;
#1899 = CARTESIAN_POINT ( 'NONE',  ( -83.77821517812500929, -32.42812499938548854, 102.3871387122750889 ) ) ;
#1900 = CARTESIAN_POINT ( 'NONE',  ( 82.39076102795759482, -31.99999999999997158, 97.13047754280712809 ) ) ;
#1901 = CARTESIAN_POINT ( 'NONE',  ( 85.15643035624999868, -34.79062499938548569, 101.5914258081833879 ) ) ;
#1902 = CARTESIAN_POINT ( 'NONE',  ( 79.64356964374999848, -31.82812499938548356, -99.99999999999998579 ) ) ;
#1903 = CARTESIAN_POINT ( 'NONE',  ( 229.8435696437499871, -31.00312499938547361, -48.40857419181671162 ) ) ;
#1904 = CARTESIAN_POINT ( 'NONE',  ( -83.77821517812500929, -34.22812499938549280, 102.3871387122750889 ) ) ;
#1905 = CARTESIAN_POINT ( 'NONE',  ( -85.15643035625001289, -33.40312499938548285, -99.99999999999998579 ) ) ;
#1906 = ORIENTED_EDGE ( 'NONE', *, *, #15604, .F. ) ;
#1907 = CARTESIAN_POINT ( 'NONE',  ( 79.64356964375001269, -33.66562499938549280, 98.40857419181659793 ) ) ;
#1908 = CARTESIAN_POINT ( 'NONE',  ( 235.5999999999999943, -34.23749999999999716, 98.26794919243110371 ) ) ;
#1909 = CARTESIAN_POINT ( 'NONE',  ( -85.15643035624999868, -35.16562499938547859, 101.5914258081833879 ) ) ;
#1910 =( BOUNDED_CURVE ( )  B_SPLINE_CURVE ( 2, ( #13585, #7248, #4614, #10570, #226, #1587, #9190, #8810, #14765 ),
 .UNSPECIFIED., .F., .F. ) 
 B_SPLINE_CURVE_WITH_KNOTS ( ( 3, 2, 2, 2, 3 ),
 ( 0.6875000000000000000, 0.6944444444444444198, 0.7083333333333333703, 0.7222222222222222099, 0.7291666666666667407 ),
 .UNSPECIFIED. ) 
 CURVE ( )  GEOMETRIC_REPRESENTATION_ITEM ( )  RATIONAL_B_SPLINE_CURVE ( ( 0.9330127018922194093, 0.9330127018922194093, 1.000000000000000000, 0.8660254037844387076, 1.000000000000000000, 0.8660254037844387076, 1.000000000000000000, 0.9330127018922187432, 0.9330127018922192983 ) ) 
 REPRESENTATION_ITEM ( '' )  );
#1911 = CARTESIAN_POINT ( 'NONE',  ( 83.20384757729335945, -33.00134618820329990, 96.99999999999997158 ) ) ;
#1912 = ORIENTED_EDGE ( 'NONE', *, *, #14250, .T. ) ;
#1913 = CARTESIAN_POINT ( 'NONE',  ( -80.90000000000000568, -30.60000000000000142, -102.5980762113533018 ) ) ;
#1914 = CARTESIAN_POINT ( 'NONE',  ( 79.39999999999999147, -34.31250000000000000, -101.7320508075688537 ) ) ;
#1915 = CARTESIAN_POINT ( 'NONE',  ( -1.391697335622809950, -4.043246145443391448, -3.503898532754372575 ) ) ;
#1916 = CARTESIAN_POINT ( 'NONE',  ( -79.64356964375001269, -34.94062499938549138, -101.5914258081833879 ) ) ;
#1917 = CARTESIAN_POINT ( 'NONE',  ( 232.5999999999999375, -32.98124999877095576, -47.00000000000011369 ) ) ;
#1918 = CARTESIAN_POINT ( 'NONE',  ( 235.3564303562499447, -33.59062499938548285, 98.40857419181659793 ) ) ;
#1919 = CARTESIAN_POINT ( 'NONE',  ( -85.40000000000000568, -33.96018749875868536, 101.7320508075688679 ) ) ;
#1920 = EDGE_LOOP ( 'NONE', ( #12424, #7805, #6513, #15193 ) ) ;
#1921 = CARTESIAN_POINT ( 'NONE',  ( 244.7999999999999545, -35.00000000000000000, 150.0000000000000000 ) ) ;
#1922 = CARTESIAN_POINT ( 'NONE',  ( 83.20384757729335945, -34.40759618943233988, -102.9999999999999858 ) ) ;
#1923 = CARTESIAN_POINT ( 'NONE',  ( 229.9620029755566293, -32.00000000000000711, 99.18121545504293124 ) ) ;
#1924 = DIRECTION ( 'NONE',  ( 0.000000000000000000, 0.000000000000000000, -1.000000000000000000 ) ) ;
#1925 = DIRECTION ( 'NONE',  ( -1.000000000000000000, 0.000000000000000000, 0.000000000000000000 ) ) ;
#1926 = CARTESIAN_POINT ( 'NONE',  ( 81.02178482187500208, -31.30312499938548498, -97.61286128772489690 ) ) ;
#1927 = DIRECTION ( 'NONE',  ( -0.000000000000000000, -1.000000000000000000, -0.000000000000000000 ) ) ;
#1928 = EDGE_CURVE ( 'NONE', #11038, #13093, #7368, .T. ) ;
#1929 = VECTOR ( 'NONE', #11797, 1000.000000000000000 ) ;
#1930 = AXIS2_PLACEMENT_3D ( 'NONE', #14747, #4304, #7423 ) ;
#1931 = ORIENTED_EDGE ( 'NONE', *, *, #704, .T. ) ;
#1932 = CARTESIAN_POINT ( 'NONE',  ( 231.2217848218749339, -33.02812499938547575, -52.38713871227520968 ) ) ;
#1933 = DIRECTION ( 'NONE',  ( 0.000000000000000000, 0.000000000000000000, 1.000000000000000000 ) ) ;
#1934 = CARTESIAN_POINT ( 'NONE',  ( 232.5999999999999375, -32.61562499938548143, 96.81714838363319586 ) ) ;
#1935 = CARTESIAN_POINT ( 'NONE',  ( 231.2217848218749339, -31.22812499938547859, -52.38713871227520968 ) ) ;
#1936 = CARTESIAN_POINT ( 'NONE',  ( -79.64356964375001269, -34.00312499938549138, 101.5914258081833879 ) ) ;
#1937 = CARTESIAN_POINT ( 'NONE',  ( -79.39999999999999147, -32.96250000000000568, -98.26794919243113213 ) ) ;
#1938 = ORIENTED_EDGE ( 'NONE', *, *, #7334, .F. ) ;
#1939 = ORIENTED_EDGE ( 'NONE', *, *, #13900, .T. ) ;
#1940 = CARTESIAN_POINT ( 'NONE',  ( 4.101954839143203912, 2.368264730583012234, -3.681130640444374436 ) ) ;
#1941 = CARTESIAN_POINT ( 'NONE',  ( 100.0000000000000000, 10.19999999999997620, -142.6499999999999773 ) ) ;
#1942 = CARTESIAN_POINT ( 'NONE',  ( -82.40000000000000568, -34.61250000000001137, 97.00000000000000000 ) ) ;
#1943 = ORIENTED_EDGE ( 'NONE', *, *, #568, .F. ) ;
#1944 = DIRECTION ( 'NONE',  ( 0.000000000000000000, 0.000000000000000000, 1.000000000000000000 ) ) ;
#1945 = CARTESIAN_POINT ( 'NONE',  ( -85.40000000000000568, -33.50624999877096855, -98.26794919243111792 ) ) ;
#1946 = COLOUR_RGB ( '',1.000000000000000000, 0.9490196078431372140, 0.9098039215686274384 ) ;
#1947 = ADVANCED_FACE ( 'NONE', ( #15175 ), #11307, .T. ) ;
#1948 = CARTESIAN_POINT ( 'NONE',  ( -3.349226789952655547, -2.685125164760744809, -0.2236248678334863682 ) ) ;
#1949 = CARTESIAN_POINT ( 'NONE',  ( -80.90000000000000568, -32.79374999877096997, 97.40192378864668399 ) ) ;
#1950 =( BOUNDED_CURVE ( )  B_SPLINE_CURVE ( 2, ( #5196, #14451, #9585, #712, #9979, #17110, #8312, #2349, #4017 ),
 .UNSPECIFIED., .F., .F. ) 
 B_SPLINE_CURVE_WITH_KNOTS ( ( 3, 2, 2, 2, 3 ),
 ( 0.2708333333333333703, 0.2777777777777777901, 0.2916666666666666852, 0.3055555555555555802, 0.3125000000000001665 ),
 .UNSPECIFIED. ) 
 CURVE ( )  GEOMETRIC_REPRESENTATION_ITEM ( )  RATIONAL_B_SPLINE_CURVE ( ( 0.9330127018922194093, 0.9330127018922196314, 1.000000000000000000, 0.8660254037844387076, 1.000000000000000000, 0.8660254037844387076, 1.000000000000000000, 0.9330127018922177440, 0.9330127018922194093 ) ) 
 REPRESENTATION_ITEM ( '' )  );
#1951 = CARTESIAN_POINT ( 'NONE',  ( -79.39999999999999147, -33.35624999877097707, 101.7320508075688537 ) ) ;
#1952 = CARTESIAN_POINT ( 'NONE',  ( -83.20384757729337366, -32.15759618943233278, 103.0000000000000000 ) ) ;
#1953 = CARTESIAN_POINT ( 'NONE',  ( 231.0999999999999375, -33.91874999877096286, -47.40192378864679768 ) ) ;
#1954 = CARTESIAN_POINT ( 'NONE',  ( 4.180345304246198879, 4.135116856707396593, -0.02129519942689974202 ) ) ;
#1955 = CARTESIAN_POINT ( 'NONE',  ( 231.2217848218749339, -34.71562499938547575, 97.61286128772489690 ) ) ;
#1956 = EDGE_CURVE ( 'NONE', #3617, #7647, #16390, .T. ) ;
#1957 = ORIENTED_EDGE ( 'NONE', *, *, #1592, .T. ) ;
#1958 = FILL_AREA_STYLE_COLOUR ( '', #14898 ) ;
#1959 = CARTESIAN_POINT ( 'NONE',  ( -85.15643035624999868, -34.67812499938548143, -101.5914258081833879 ) ) ;
#1960 = DIRECTION ( 'NONE',  ( -0.8191520442889902442, 0.000000000000000000, -0.5735764363510482688 ) ) ;
#1961 = AXIS2_PLACEMENT_3D ( 'NONE', #12311, #3512, #5181 ) ;
#1962 = ORIENTED_EDGE ( 'NONE', *, *, #11514, .F. ) ;
#1963 = B_SPLINE_CURVE_WITH_KNOTS ( 'NONE', 3,
 ( #14159, #9866, #2440, #3801, #15539, #793, #3611, #6750, #16907, #15731, #15438, #2154, #6850, #15827, #18670, #11130, #12795, #5286 ),
 .UNSPECIFIED., .F., .F.,
 ( 4, 2, 2, 2, 2, 2, 2, 2, 4 ),
 ( 0.000000000000000000, 0.0007106627595359821031, 0.001421325519071964206, 0.002131988278607946201, 0.002842651038143928412, 0.003553313797679910624, 0.004263976557215892402, 0.004974639316751875047, 0.005685302076287856825 ),
 .UNSPECIFIED. ) ;
#1964 = LINE ( 'NONE', #3430, #1165 ) ;
#1965 = DIRECTION ( 'NONE',  ( 1.000000000000000000, 0.000000000000000000, 0.000000000000000000 ) ) ;
#1966 = UNCERTAINTY_MEASURE_WITH_UNIT (LENGTH_MEASURE( 1.000000000000000082E-05 ), #9972, 'distance_accuracy_value', 'NONE');
#1967 = FACE_OUTER_BOUND ( 'NONE', #16196, .T. ) ;
#1968 = ORIENTED_EDGE ( 'NONE', *, *, #4522, .T. ) ;
#1969 = DIRECTION ( 'NONE',  ( -0.000000000000000000, -1.000000000000000000, -0.000000000000000000 ) ) ;
#1970 = VERTEX_POINT ( 'NONE', #12154 ) ;
#1971 = VERTEX_POINT ( 'NONE', #6206 ) ;
#1972 = CARTESIAN_POINT ( 'NONE',  ( 80.90000000000000568, -34.74374999877097281, 97.40192378864668399 ) ) ;
#1973 = CARTESIAN_POINT ( 'NONE',  ( 79.39999999999999147, -30.71250000000000568, -101.7320508075688537 ) ) ;
#1974 = CARTESIAN_POINT ( 'NONE',  ( -82.40000000000000568, -30.00000000000000355, -99.99999999999998579 ) ) ;
#1975 = ADVANCED_FACE ( 'NONE', ( #12053 ), #14887, .F. ) ;
#1976 = CARTESIAN_POINT ( 'NONE',  ( -82.39999999999999147, -33.65624999877096712, 96.53589838486223584 ) ) ;
#1977 = CARTESIAN_POINT ( 'NONE',  ( 96.99999999999994316, -21.80000000000003268, -137.3499999999999943 ) ) ;
#1978 = CARTESIAN_POINT ( 'NONE',  ( 105.1999999999999744, -4.999999999999976907, 153.0000000000000000 ) ) ;
#1979 = CARTESIAN_POINT ( 'NONE',  ( 79.64356964374999848, -32.72812499938548569, -99.99999999999998579 ) ) ;
#1980 = CARTESIAN_POINT ( 'NONE',  ( -81.59615242270662350, -32.06115380933863435, -96.99999999999997158 ) ) ;
#1981 = CARTESIAN_POINT ( 'NONE',  ( -83.77821517812500929, -33.66562499938548569, 102.3871387122750889 ) ) ;
#1982 = CARTESIAN_POINT ( 'NONE',  ( 85.15643035624999868, -33.25312499938548427, -101.5914258081833879 ) ) ;
#1983 = ORIENTED_EDGE ( 'NONE', *, *, #6152, .T. ) ;
#1984 = CARTESIAN_POINT ( 'NONE',  ( 232.5999999999999375, -32.36249999999999716, -53.46410161513786363 ) ) ;
#1985 = CARTESIAN_POINT ( 'NONE',  ( -79.39999999999999147, -33.37500000000000000, 99.99999999999998579 ) ) ;
#1986 =( BOUNDED_CURVE ( )  B_SPLINE_CURVE ( 2, ( #1738, #15028, #1650, #10629, #16594, #9349, #14039, #8182, #6340 ),
 .UNSPECIFIED., .F., .F. ) 
 B_SPLINE_CURVE_WITH_KNOTS ( ( 3, 2, 2, 2, 3 ),
 ( 0.4791666666666666297, 0.4861111111111111049, 0.5000000000000000000, 0.5138888888888888395, 0.5208333333333333703 ),
 .UNSPECIFIED. ) 
 CURVE ( )  GEOMETRIC_REPRESENTATION_ITEM ( )  RATIONAL_B_SPLINE_CURVE ( ( 0.9330127018922194093, 0.9330127018922190762, 1.000000000000000000, 0.8660254037844387076, 1.000000000000000000, 0.8660254037844387076, 1.000000000000000000, 0.9330127018922187432, 0.9330127018922192983 ) ) 
 REPRESENTATION_ITEM ( '' )  );
#1987 = CARTESIAN_POINT ( 'NONE',  ( 85.40000000000000568, -33.54374999877096286, -99.99999999999998579 ) ) ;
#1988 = CARTESIAN_POINT ( 'NONE',  ( 229.8435696437499587, -32.54062499938547859, 98.40857419181659793 ) ) ;
#1989 = CARTESIAN_POINT ( 'NONE',  ( -83.77821517812500929, -31.22812499938548569, 97.61286128772489690 ) ) ;
#1990 = ADVANCED_FACE ( 'NONE', ( #6104 ), #55, .F. ) ;
#1991 = CARTESIAN_POINT ( 'NONE',  ( 235.3564303562499447, -32.31562499938547717, -48.40857419181671162 ) ) ;
#1992 = CARTESIAN_POINT ( 'NONE',  ( -85.40000000000000568, -32.21249999999999858, 101.7320508075688679 ) ) ;
#1993 = ORIENTED_EDGE ( 'NONE', *, *, #4541, .T. ) ;
#1994 = CARTESIAN_POINT ( 'NONE',  ( -84.50041942204053669, -34.99839409658486034, 102.1701536479666999 ) ) ;
#1995 = CARTESIAN_POINT ( 'NONE',  ( 232.5999999999999375, -29.99999999999999645, -50.00000000000011369 ) ) ;
#1996 = CARTESIAN_POINT ( 'NONE',  ( 83.77821517812500929, -32.91562499938547859, 102.3871387122750889 ) ) ;
#1997 = CARTESIAN_POINT ( 'NONE',  ( 84.44763168836730927, -32.00000000000000711, -101.8452947671444093 ) ) ;
#1998 = CARTESIAN_POINT ( 'NONE',  ( -81.02178482187500208, -30.85312499938548569, 97.61286128772489690 ) ) ;
#1999 = CARTESIAN_POINT ( 'NONE',  ( -85.15643035625001289, -32.09062499938548996, -101.5914258081833879 ) ) ;
#2000 = CARTESIAN_POINT ( 'NONE',  ( 85.15643035625001289, -30.14062499938548711, 99.99999999999998579 ) ) ;
#2001 = CARTESIAN_POINT ( 'NONE',  ( 82.39999999999999147, -31.04062499938548569, -103.1828516163667899 ) ) ;
#2002 = CARTESIAN_POINT ( 'NONE',  ( -79.64356964374998427, -33.66562499938548569, 101.5914258081833879 ) ) ;
#2003 = CARTESIAN_POINT ( 'NONE',  ( -81.02178482187500208, -34.60312499938549280, -97.61286128772489690 ) ) ;
#2004 = VERTEX_POINT ( 'NONE', #1516 ) ;
#2005 = CARTESIAN_POINT ( 'NONE',  ( 82.39999999999999147, -33.74062499938548854, 96.81714838363319586 ) ) ;
#2006 = CARTESIAN_POINT ( 'NONE',  ( 235.5999999999999943, -34.31249999999999289, 101.7320508075688537 ) ) ;
#2007 = CARTESIAN_POINT ( 'NONE',  ( -79.64356964375001269, -30.40312499938548285, 101.5914258081833879 ) ) ;
#2008 = CARTESIAN_POINT ( 'NONE',  ( -81.02178482187500208, -34.15312499938548285, 102.3871387122750889 ) ) ;
#2009 = CARTESIAN_POINT ( 'NONE',  ( -82.39999999999999147, -33.48750000000000426, 103.0000000000000000 ) ) ;
#2010 = ORIENTED_EDGE ( 'NONE', *, *, #7677, .T. ) ;
#2011 = CARTESIAN_POINT ( 'NONE',  ( -85.40000000000000568, -32.73750000000000426, -101.7320508075688679 ) ) ;
#2012 = CARTESIAN_POINT ( 'NONE',  ( 229.5999999999999375, -34.44374999877096144, -50.00000000000011369 ) ) ;
#2013 = CARTESIAN_POINT ( 'NONE',  ( -2.804994570502171047, -3.229033611042465335, -3.526374918436838701 ) ) ;
#2014 = CARTESIAN_POINT ( 'NONE',  ( -79.39999999999999147, -32.83124999877097139, 98.26794919243110371 ) ) ;
#2015 = CARTESIAN_POINT ( 'NONE',  ( 229.8435696437499303, -33.85312499938548569, 99.99999999999998579 ) ) ;
#2016 = CARTESIAN_POINT ( 'NONE',  ( -82.39999999999999147, -34.33518749875868536, 103.4641016151377499 ) ) ;
#2017 = ORIENTED_EDGE ( 'NONE', *, *, #1497, .F. ) ;
#2018 = DIRECTION ( 'NONE',  ( 1.000000000000000000, -1.387778780781445676E-15, -2.407412430484046130E-31 ) ) ;
#2019 = DIRECTION ( 'NONE',  ( 0.000000000000000000, 0.000000000000000000, 1.000000000000000000 ) ) ;
#2020 = CARTESIAN_POINT ( 'NONE',  ( 230.5523683116323355, -32.00000000000000000, 101.8452947671440540 ) ) ;
#2021 = FACE_OUTER_BOUND ( 'NONE', #18994, .T. ) ;
#2022 = CARTESIAN_POINT ( 'NONE',  ( -83.20384757729338787, -34.53615380933862866, 97.00000000000000000 ) ) ;
#2023 = CARTESIAN_POINT ( 'NONE',  ( 83.77821517812500929, -32.57812499938548711, -97.61286128772489690 ) ) ;
#2024 = CARTESIAN_POINT ( 'NONE',  ( 232.5999999999999375, -32.36249999999999716, -53.00000000000011369 ) ) ;
#2025 = AXIS2_PLACEMENT_3D ( 'NONE', #9054, #13641, #184 ) ;
#2026 = EDGE_LOOP ( 'NONE', ( #49, #19244, #4813, #12099, #5239 ) ) ;
#2027 =( BOUNDED_CURVE ( )  B_SPLINE_CURVE ( 2, ( #6368, #16717, #14070, #4902, #16912, #6560, #12508, #18475, #5189 ),
 .UNSPECIFIED., .F., .F. ) 
 B_SPLINE_CURVE_WITH_KNOTS ( ( 3, 2, 2, 2, 3 ),
 ( 0.4374999999999999445, 0.4444444444444444198, 0.4583333333333333148, 0.4722222222222222099, 0.4791666666666666297 ),
 .UNSPECIFIED. ) 
 CURVE ( )  GEOMETRIC_REPRESENTATION_ITEM ( )  RATIONAL_B_SPLINE_CURVE ( ( 0.9330127018922192983, 0.9330127018922187432, 1.000000000000000000, 0.8660254037844387076, 1.000000000000000000, 0.8660254037844387076, 1.000000000000000000, 0.9330127018922196314, 0.9330127018922194093 ) ) 
 REPRESENTATION_ITEM ( '' )  );
#2028 = CARTESIAN_POINT ( 'NONE',  ( 85.40000000000000568, -30.80624999877096926, 98.26794919243111792 ) ) ;
#2029 = PRODUCT_CONTEXT ( 'NONE', #3323, 'mechanical' ) ;
#2030 = CARTESIAN_POINT ( 'NONE',  ( 232.5999999999999375, -33.06562499938547717, 96.81714838363319586 ) ) ;
#2031 = CARTESIAN_POINT ( 'NONE',  ( 235.3564303562499447, -30.96562499938547930, -48.40857419181671162 ) ) ;
#2032 = CARTESIAN_POINT ( 'NONE',  ( -79.64356964374999848, -33.06562499938548427, 99.99999999999998579 ) ) ;
#2033 = CARTESIAN_POINT ( 'NONE',  ( 235.5999999999999375, -34.72499999999999432, -50.00000000000011369 ) ) ;
#2034 = VERTEX_POINT ( 'NONE', #18121 ) ;
#2035 = ORIENTED_EDGE ( 'NONE', *, *, #14754, .F. ) ;
#2036 = CARTESIAN_POINT ( 'NONE',  ( -79.64356964374999848, -30.81562499938548427, -99.99999999999998579 ) ) ;
#2037 = CARTESIAN_POINT ( 'NONE',  ( -85.40000000000000568, -30.80624999877096570, 101.7320508075688821 ) ) ;
#2038 = PLANE ( 'NONE',  #2554 ) ;
#2039 = EDGE_CURVE ( 'NONE', #3376, #2644, #2875, .T. ) ;
#2040 = ORIENTED_EDGE ( 'NONE', *, *, #9112, .T. ) ;
#2041 = CARTESIAN_POINT ( 'NONE',  ( 79.64356964374998427, -32.31562499938548427, 98.40857419181659793 ) ) ;
#2042 = CARTESIAN_POINT ( 'NONE',  ( -79.39999999999999147, -33.73124999877096997, -101.7320508075688821 ) ) ;
#2043 = AXIS2_PLACEMENT_3D ( 'NONE', #5454, #6912, #18832 ) ;
#2044 = CARTESIAN_POINT ( 'NONE',  ( -82.65333140691201663, -34.99995246259153703, 97.01071553687880566 ) ) ;
#2045 = CARTESIAN_POINT ( 'NONE',  ( -85.40000000000000568, -33.05624999877096570, 101.7320508075688679 ) ) ;
#2046 = CARTESIAN_POINT ( 'NONE',  ( -82.39999999999999147, -35.00624999877097565, 96.53589838486223584 ) ) ;
#2047 = CARTESIAN_POINT ( 'NONE',  ( 83.43443729601675329, -34.99999999999999289, -102.5775038898419496 ) ) ;
#2048 = CARTESIAN_POINT ( 'NONE',  ( 232.5999999999999091, -34.10624999877096286, -53.00000000000010658 ) ) ;
#2049 = DIRECTION ( 'NONE',  ( -0.000000000000000000, -0.000000000000000000, 1.000000000000000000 ) ) ;
#2050 = CARTESIAN_POINT ( 'NONE',  ( 233.9782151781249411, -34.94062499938547717, 102.3871387122750889 ) ) ;
#2051 = ORIENTED_EDGE ( 'NONE', *, *, #2656, .F. ) ;
#2052 = SURFACE_STYLE_FILL_AREA ( #12504 ) ;
#2053 = LINE ( 'NONE', #5291, #15203 ) ;
#2054 = CARTESIAN_POINT ( 'NONE',  ( 4.175813232069148562, 4.122719923832742772, -5.545971589517866732E-16 ) ) ;
#2055 = EDGE_LOOP ( 'NONE', ( #11819, #10542, #1398, #11442 ) ) ;
#2056 = CIRCLE ( 'NONE', #7671, 2.649999999999985700 ) ;
#2057 = CARTESIAN_POINT ( 'NONE',  ( -83.20384757729335945, -33.45134618820330985, 102.9999999999999858 ) ) ;
#2058 = CARTESIAN_POINT ( 'NONE',  ( -85.40000000000000568, -30.39374999877097139, 99.99999999999998579 ) ) ;
#2059 = CARTESIAN_POINT ( 'NONE',  ( 2.855764796983346177, -2.970025579236428737, -0.09382832055446485575 ) ) ;
#2060 = ORIENTED_EDGE ( 'NONE', *, *, #1928, .T. ) ;
#2061 = CARTESIAN_POINT ( 'NONE',  ( 25.60000000000000142, 0.000000000000000000, 0.000000000000000000 ) ) ;
#2062 = ADVANCED_FACE ( 'NONE', ( #16556 ), #16458, .F. ) ;
#2063 = ORIENTED_EDGE ( 'NONE', *, *, #17735, .T. ) ;
#2064 = ORIENTED_EDGE ( 'NONE', *, *, #8892, .T. ) ;
#2065 =( BOUNDED_CURVE ( )  B_SPLINE_CURVE ( 2, ( #8023, #432, #13983, #6377, #12426, #6569, #18394, #2169, #11050 ),
 .UNSPECIFIED., .F., .F. ) 
 B_SPLINE_CURVE_WITH_KNOTS ( ( 3, 2, 2, 2, 3 ),
 ( 0.6041666666666667407, 0.6111111111111111605, 0.6250000000000000000, 0.6388888888888888395, 0.6458333333333332593 ),
 .UNSPECIFIED. ) 
 CURVE ( )  GEOMETRIC_REPRESENTATION_ITEM ( )  RATIONAL_B_SPLINE_CURVE ( ( 0.9330127018922192983, 0.9330127018922198534, 1.000000000000000000, 0.8660254037844387076, 1.000000000000000000, 0.8660254037844387076, 1.000000000000000000, 0.9330127018922198534, 0.9330127018922192983 ) ) 
 REPRESENTATION_ITEM ( '' )  );
#2066 = CARTESIAN_POINT ( 'NONE',  ( 81.02178482187500208, -34.49062499938548854, -102.3871387122750889 ) ) ;
#2067 = CARTESIAN_POINT ( 'NONE',  ( -79.64356964374998427, -34.94062499938548427, -101.5914258081833879 ) ) ;
#2068 = AXIS2_PLACEMENT_3D ( 'NONE', #200, #12101, #18075 ) ;
#2069 = ADVANCED_FACE ( 'NONE', ( #3157 ), #11955, .T. ) ;
#2070 = CARTESIAN_POINT ( 'NONE',  ( -85.40000000000000568, -34.03124999877096712, 98.26794919243111792 ) ) ;
#2071 = CARTESIAN_POINT ( 'NONE',  ( -85.40000000000000568, -34.00856250001229597, 101.7320508075688679 ) ) ;
#2072 = CARTESIAN_POINT ( 'NONE',  ( -79.39999999999999147, -33.28124999877096712, 98.26794919243110371 ) ) ;
#2073 = LINE ( 'NONE', #8030, #8496 ) ;
#2074 = CIRCLE ( 'NONE', #1143, 3.000000000000002665 ) ;
#2075 = CARTESIAN_POINT ( 'NONE',  ( 79.64356964374998427, -33.21562499938548996, -101.5914258081833879 ) ) ;
#2076 = CARTESIAN_POINT ( 'NONE',  ( 82.40000000000000568, -33.93750000000000711, 97.00000000000000000 ) ) ;
#2077 = CARTESIAN_POINT ( 'NONE',  ( -83.77821517812500929, -32.01562499938548001, 97.61286128772489690 ) ) ;
#2078 = CARTESIAN_POINT ( 'NONE',  ( 81.02178482187500208, -33.44062499938548427, -97.61286128772489690 ) ) ;
#2079 = ORIENTED_EDGE ( 'NONE', *, *, #8174, .T. ) ;
#2080 = CARTESIAN_POINT ( 'NONE',  ( 229.5999999999999375, -32.28750000000000142, -51.73205080756898866 ) ) ;
#2081 = CARTESIAN_POINT ( 'NONE',  ( -79.39999999999999147, -33.33749999999999858, 98.26794919243110371 ) ) ;
#2082 = CARTESIAN_POINT ( 'NONE',  ( -83.90000000000000568, -31.21874999877097068, -97.40192378864668399 ) ) ;
#2083 = ADVANCED_FACE ( 'NONE', ( #19301 ), #6298, .F. ) ;
#2084 = CARTESIAN_POINT ( 'NONE',  ( 82.39999999999999147, -33.65624999877097423, -97.00000000000000000 ) ) ;
#2085 = CARTESIAN_POINT ( 'NONE',  ( 229.8435696437499303, -32.95312499938548001, 99.99999999999998579 ) ) ;
#2086 = CARTESIAN_POINT ( 'NONE',  ( -85.15643035625001289, -30.70312499938548711, 99.99999999999998579 ) ) ;
#2087 = CARTESIAN_POINT ( 'NONE',  ( 235.3564303562499447, -32.72812499938547859, -50.00000000000011369 ) ) ;
#2088 = EDGE_CURVE ( 'NONE', #3907, #1884, #3065, .T. ) ;
#2089 = CARTESIAN_POINT ( 'NONE',  ( -80.90000000000000568, -31.94999999999999929, 97.40192378864668399 ) ) ;
#2090 = ORIENTED_EDGE ( 'NONE', *, *, #7559, .F. ) ;
#2091 = CARTESIAN_POINT ( 'NONE',  ( 232.5999999999999375, -33.71249999999999147, -53.00000000000010658 ) ) ;
#2092 = CARTESIAN_POINT ( 'NONE',  ( 82.39999999999999147, -33.17812499938548854, 96.81714838363319586 ) ) ;
#2093 = AXIS2_PLACEMENT_3D ( 'NONE', #15295, #8948, #3277 ) ;
#2094 = CARTESIAN_POINT ( 'NONE',  ( 0.000000000000000000, 0.000000000000000000, -0.3080913168122742518 ) ) ;
#2095 = CARTESIAN_POINT ( 'NONE',  ( -85.15643035625001289, -30.70312499938548711, 99.99999999999998579 ) ) ;
#2096 = AXIS2_PLACEMENT_3D ( 'NONE', #13867, #12506, #8011 ) ;
#2097 = DIRECTION ( 'NONE',  ( 1.000000000000000000, 0.000000000000000000, 0.000000000000000000 ) ) ;
#2098 = CARTESIAN_POINT ( 'NONE',  ( 85.15643035625001289, -31.49062499938548498, 99.99999999999998579 ) ) ;
#2099 =( BOUNDED_CURVE ( )  B_SPLINE_CURVE ( 2, ( #18299, #626, #17023, #12431, #18693, #6574, #14179, #12522, #12619 ),
 .UNSPECIFIED., .F., .F. ) 
 B_SPLINE_CURVE_WITH_KNOTS ( ( 3, 2, 2, 2, 3 ),
 ( 0.3958333333333334259, 0.4027777777777777901, 0.4166666666666666852, 0.4305555555555555802, 0.4375000000000000555 ),
 .UNSPECIFIED. ) 
 CURVE ( )  GEOMETRIC_REPRESENTATION_ITEM ( )  RATIONAL_B_SPLINE_CURVE ( ( 0.9330127018922192983, 0.9330127018922200755, 1.000000000000000000, 0.8660254037844387076, 1.000000000000000000, 0.8660254037844387076, 1.000000000000000000, 0.9330127018922187432, 0.9330127018922192983 ) ) 
 REPRESENTATION_ITEM ( '' )  );
#2100 = CARTESIAN_POINT ( 'NONE',  ( 83.77821517812500929, -31.97812499938548925, -102.3871387122750889 ) ) ;
#2101 = CARTESIAN_POINT ( 'NONE',  ( 232.5999999999999375, -32.81249999999999289, -53.00000000000011369 ) ) ;
#2102 = CARTESIAN_POINT ( 'NONE',  ( -81.02178482187500208, -34.45312499938548711, 97.61286128772489690 ) ) ;
#2103 = CARTESIAN_POINT ( 'NONE',  ( -85.15643035624999868, -32.91562499938549280, -98.40857419181659793 ) ) ;
#2104 = ORIENTED_EDGE ( 'NONE', *, *, #12723, .T. ) ;
#2105 = CARTESIAN_POINT ( 'NONE',  ( 81.02178482187500208, -33.10312499938548569, 102.3871387122750889 ) ) ;
#2106 = AXIS2_PLACEMENT_3D ( 'NONE', #14519, #11790, #4559 ) ;
#2107 = CARTESIAN_POINT ( 'NONE',  ( 4.180345304246200655, -4.135116856707401922, 0.02129519942689706707 ) ) ;
#2108 = CARTESIAN_POINT ( 'NONE',  ( -82.39999999999999147, -31.60312499938548569, 96.81714838363319586 ) ) ;
#2109 = CARTESIAN_POINT ( 'NONE',  ( -79.64356964375001269, -33.14062499938548711, 98.40857419181659793 ) ) ;
#2110 = CARTESIAN_POINT ( 'NONE',  ( -2.000000000000007550, -3.464101615137749945, 0.000000000000000000 ) ) ;
#2111 = EDGE_LOOP ( 'NONE', ( #18672, #110, #18684, #7941 ) ) ;
#2112 = ADVANCED_FACE ( 'NONE', ( #9027 ), #3827, .T. ) ;
#2113 = CARTESIAN_POINT ( 'NONE',  ( -79.39999999999999147, -33.41250000000000142, -98.26794919243113213 ) ) ;
#2114 = AXIS2_PLACEMENT_3D ( 'NONE', #19302, #11861, #16360 ) ;
#2115 = STYLED_ITEM ( 'NONE', ( #2752 ), #5334 ) ;
#2116 = LINE ( 'NONE', #15402, #14711 ) ;
#2117 = CARTESIAN_POINT ( 'NONE',  ( 84.70388354820684640, -35.00002705695777649, -98.07851859032987818 ) ) ;
#2118 = CARTESIAN_POINT ( 'NONE',  ( -85.15643035625001289, -35.20312499938548711, -99.99999999999998579 ) ) ;
#2119 = CARTESIAN_POINT ( 'NONE',  ( 233.9782151781249411, -34.60312499938548569, 102.3871387122750889 ) ) ;
#2120 = CARTESIAN_POINT ( 'NONE',  ( -82.39999999999999147, -34.56018749875867258, 96.53589838486223584 ) ) ;
#2121 = AXIS2_PLACEMENT_3D ( 'NONE', #12853, #8358, #12655 ) ;
#2122 = ORIENTED_EDGE ( 'NONE', *, *, #2958, .F. ) ;
#2123 = EDGE_CURVE ( 'NONE', #3130, #11060, #14746, .T. ) ;
#2124 = DIRECTION ( 'NONE',  ( 0.000000000000000000, 0.000000000000000000, 1.000000000000000000 ) ) ;
#2125 = FACE_OUTER_BOUND ( 'NONE', #6248, .T. ) ;
#2126 = CARTESIAN_POINT ( 'NONE',  ( 230.1427008797911640, -31.99999999999999289, 101.2614033343866424 ) ) ;
#2127 = CARTESIAN_POINT ( 'NONE',  ( 232.5999999999999375, -33.88124999877096855, 103.0000000000000000 ) ) ;
#2128 = DIRECTION ( 'NONE',  ( -0.000000000000000000, -1.000000000000000000, -0.000000000000000000 ) ) ;
#2129 = CARTESIAN_POINT ( 'NONE',  ( 81.02178482187500208, -30.40312499938548640, -97.61286128772489690 ) ) ;
#2130 = VECTOR ( 'NONE', #16619, 1000.000000000000000 ) ;
#2131 = CARTESIAN_POINT ( 'NONE',  ( 231.6691923799541826, -35.05289549976082952, 96.44210921874548603 ) ) ;
#2132 = CIRCLE ( 'NONE', #18054, 4.000000000000000000 ) ;
#2133 = ORIENTED_EDGE ( 'NONE', *, *, #8502, .T. ) ;
#2134 = CARTESIAN_POINT ( 'NONE',  ( 83.90000000000000568, -30.46874999877096712, 102.5980762113533018 ) ) ;
#2135 = SHAPE_DEFINITION_REPRESENTATION ( #13860, #16991 ) ;
#2136 = CARTESIAN_POINT ( 'NONE',  ( 232.5999999999999375, -31.49062499938547788, 103.1828516163667899 ) ) ;
#2137 = CARTESIAN_POINT ( 'NONE',  ( 229.5999999999999375, -34.85624999877096286, -48.26794919243123161 ) ) ;
#2138 = CARTESIAN_POINT ( 'NONE',  ( -79.64356964375001269, -34.45312499938548711, 101.5914258081833879 ) ) ;
#2139 = CARTESIAN_POINT ( 'NONE',  ( -82.39999999999999147, -34.83749999999999858, 103.0000000000000000 ) ) ;
#2140 = ORIENTED_EDGE ( 'NONE', *, *, #19313, .T. ) ;
#2141 = ORIENTED_EDGE ( 'NONE', *, *, #18816, .T. ) ;
#2142 = CARTESIAN_POINT ( 'NONE',  ( -82.39999999999999147, -32.05312499938548854, -103.1828516163667899 ) ) ;
#2143 = CARTESIAN_POINT ( 'NONE',  ( -79.39999999999999147, -33.80624999877097281, -98.26794919243113213 ) ) ;
#2144 = ORIENTED_EDGE ( 'NONE', *, *, #15355, .F. ) ;
#2145 = CARTESIAN_POINT ( 'NONE',  ( 85.15643035625001289, -34.71562499938548285, 98.40857419181659793 ) ) ;
#2146 = CARTESIAN_POINT ( 'NONE',  ( -82.39999999999999147, -34.10624999877096997, -103.4641016151377499 ) ) ;
#2147 = VECTOR ( 'NONE', #5552, 1000.000000000000000 ) ;
#2148 = CARTESIAN_POINT ( 'NONE',  ( 79.39999999999999147, -31.08750000000000213, 101.7320508075688821 ) ) ;
#2149 = CARTESIAN_POINT ( 'NONE',  ( 110.0000000000000000, 10.19999999999997620, -150.0000000000000000 ) ) ;
#2150 = CARTESIAN_POINT ( 'NONE',  ( -79.39999999999999147, -31.48124999877097352, 98.26794919243110371 ) ) ;
#2151 = CARTESIAN_POINT ( 'NONE',  ( -85.40000000000000568, -33.50624999877096855, 101.7320508075688679 ) ) ;
#2152 = CARTESIAN_POINT ( 'NONE',  ( 85.24876232368839624, -34.99999999999999289, -100.5466586069351393 ) ) ;
#2153 = CARTESIAN_POINT ( 'NONE',  ( 232.5999999999999659, -32.53124999877096712, 102.9999999999999858 ) ) ;
#2154 = CARTESIAN_POINT ( 'NONE',  ( 232.1383900424027900, -31.99999999999999289, 102.8104067583494157 ) ) ;
#2155 = CARTESIAN_POINT ( 'NONE',  ( 229.8435696437499871, -33.25312499938547717, 101.5914258081833879 ) ) ;
#2156 = ORIENTED_EDGE ( 'NONE', *, *, #4800, .T. ) ;
#2157 = CARTESIAN_POINT ( 'NONE',  ( -83.90000000000000568, -34.12500000000000000, 97.40192378864668399 ) ) ;
#2158 = PRESENTATION_STYLE_ASSIGNMENT (( #9576 ) ) ;
#2159 = CARTESIAN_POINT ( 'NONE',  ( 231.0999999999999375, -32.11874999877096570, 102.5980762113533018 ) ) ;
#2160 =( BOUNDED_CURVE ( )  B_SPLINE_CURVE ( 2, ( #12955, #13054, #18926, #3773, #11495, #19020, #4070, #17459, #14221 ),
 .UNSPECIFIED., .F., .F. ) 
 B_SPLINE_CURVE_WITH_KNOTS ( ( 3, 2, 2, 2, 3 ),
 ( 0.5208333333333334814, 0.5277777777777777901, 0.5416666666666666297, 0.5555555555555555802, 0.5625000000000000000 ),
 .UNSPECIFIED. ) 
 CURVE ( )  GEOMETRIC_REPRESENTATION_ITEM ( )  RATIONAL_B_SPLINE_CURVE ( ( 0.9330127018922194093, 0.9330127018922209636, 1.000000000000000000, 0.8660254037844387076, 1.000000000000000000, 0.8660254037844387076, 1.000000000000000000, 0.9330127018922194093, 0.9330127018922194093 ) ) 
 REPRESENTATION_ITEM ( '' )  );
#2161 = ORIENTED_EDGE ( 'NONE', *, *, #5204, .F. ) ;
#2162 = FACE_OUTER_BOUND ( 'NONE', #18529, .T. ) ;
#2163 = CARTESIAN_POINT ( 'NONE',  ( 246.9999999999999716, -29.80000000000000426, -100.0000000000000000 ) ) ;
#2164 = FILL_AREA_STYLE_COLOUR ( '', #10057 ) ;
#2165 = ORIENTED_EDGE ( 'NONE', *, *, #8055, .F. ) ;
#2166 = DIRECTION ( 'NONE',  ( 0.000000000000000000, 1.000000000000000000, 0.000000000000000000 ) ) ;
#2167 = CARTESIAN_POINT ( 'NONE',  ( 4.024499207728847949, -2.323545700935699454, -3.572172305156873673 ) ) ;
#2168 = ORIENTED_EDGE ( 'NONE', *, *, #14963, .T. ) ;
#2169 = CARTESIAN_POINT ( 'NONE',  ( 233.4038475772933339, -33.46740381056766012, -47.00000000000011369 ) ) ;
#2170 = CARTESIAN_POINT ( 'NONE',  ( 85.15643035624999868, -35.05312499938548143, -101.5914258081833879 ) ) ;
#2171 = DIRECTION ( 'NONE',  ( 0.000000000000000000, 0.000000000000000000, -1.000000000000000000 ) ) ;
#2172 = CARTESIAN_POINT ( 'NONE',  ( -79.39999999999999147, -35.11874999877096570, 99.99999999999998579 ) ) ;
#2173 = CARTESIAN_POINT ( 'NONE',  ( -82.39999999999999147, -30.11250000000000426, 96.53589838486223584 ) ) ;
#2174 = CARTESIAN_POINT ( 'NONE',  ( 232.5999999999999375, -32.75624999877096144, 96.99999999999998579 ) ) ;
#2175 = FILL_AREA_STYLE ('',( #18494 ) ) ;
#2176 = CARTESIAN_POINT ( 'NONE',  ( 85.15643035625001289, -32.02817623523065294, -101.0587761908874569 ) ) ;
#2177 = CARTESIAN_POINT ( 'NONE',  ( 79.39999999999999147, -33.82500000000000284, 99.99999999999998579 ) ) ;
#2178 = CARTESIAN_POINT ( 'NONE',  ( -82.39999999999999147, -34.30312499938548143, 96.81714838363319586 ) ) ;
#2179 = DIRECTION ( 'NONE',  ( -1.000000000000000000, 1.387778780781445478E-15, 2.407412430484046130E-31 ) ) ;
#2180 = ORIENTED_EDGE ( 'NONE', *, *, #14586, .T. ) ;
#2181 = CARTESIAN_POINT ( 'NONE',  ( -83.90000000000000568, -34.12500000000000000, 97.40192378864668399 ) ) ;
#2182 = EDGE_CURVE ( 'NONE', #18235, #10587, #17387, .T. ) ;
#2183 = EDGE_CURVE ( 'NONE', #17562, #4492, #18603, .T. ) ;
#2184 = CARTESIAN_POINT ( 'NONE',  ( 0.02448733951239481094, 4.877042772274728044, -3.751161874094022242 ) ) ;
#2185 = CARTESIAN_POINT ( 'NONE',  ( 232.5999999999999943, -33.29062499938547859, 103.1828516163667899 ) ) ;
#2186 = CARTESIAN_POINT ( 'NONE',  ( -85.15643035624999868, -30.29062499938548925, 98.40857419181659793 ) ) ;
#2187 = CARTESIAN_POINT ( 'NONE',  ( 233.9782151781249411, -34.90312499938547575, -52.38713871227520968 ) ) ;
#2188 = CARTESIAN_POINT ( 'NONE',  ( -83.90000000000000568, -32.17500000000000426, 102.5980762113533018 ) ) ;
#2189 = ORIENTED_EDGE ( 'NONE', *, *, #13529, .F. ) ;
#2190 = CARTESIAN_POINT ( 'NONE',  ( 3.878089031707363521, 0.7015470581927524263, 3.500000000000000444 ) ) ;
#2191 = DIRECTION ( 'NONE',  ( 0.000000000000000000, 0.000000000000000000, -1.000000000000000000 ) ) ;
#2192 = CARTESIAN_POINT ( 'NONE',  ( 79.64356964374999848, -31.71562499938548285, 99.99999999999998579 ) ) ;
#2193 = ADVANCED_FACE ( 'NONE', ( #826 ), #4930, .F. ) ;
#2194 = CARTESIAN_POINT ( 'NONE',  ( -83.77821517812500929, -34.37812499938548427, 97.61286128772489690 ) ) ;
#2195 = CARTESIAN_POINT ( 'NONE',  ( 81.01744233620654256, -32.00000000000000000, 97.41649131116879801 ) ) ;
#2196 = CARTESIAN_POINT ( 'NONE',  ( 85.15643035625001289, -32.39062499938548711, 99.99999999999998579 ) ) ;
#2197 = CARTESIAN_POINT ( 'NONE',  ( 83.77821517812500929, -30.62812499938548783, -102.3871387122750889 ) ) ;
#2198 = CARTESIAN_POINT ( 'NONE',  ( 235.3564303562499447, -32.12812499938547717, -51.59142580818350865 ) ) ;
#2199 = CARTESIAN_POINT ( 'NONE',  ( -83.77821517812500929, -30.66562499938548569, -102.3871387122750889 ) ) ;
#2200 = ADVANCED_FACE ( 'NONE', ( #18217 ), #13998, .F. ) ;
#2201 = ORIENTED_EDGE ( 'NONE', *, *, #3547, .T. ) ;
#2202 = CARTESIAN_POINT ( 'NONE',  ( 83.77821517812500929, -33.32812499938548711, 97.61286128772489690 ) ) ;
#2203 = CARTESIAN_POINT ( 'NONE',  ( 3.961551342854050528, -2.319461885623371966, -2.982574167880817750 ) ) ;
#2204 = CARTESIAN_POINT ( 'NONE',  ( -82.39999999999999147, -32.05312499938548854, 96.81714838363319586 ) ) ;
#2205 = CARTESIAN_POINT ( 'NONE',  ( -84.51154815724953551, -35.25364861271051353, 98.22820072003833047 ) ) ;
#2206 = DIRECTION ( 'NONE',  ( -0.000000000000000000, -1.000000000000000000, -0.000000000000000000 ) ) ;
#2207 = VERTEX_POINT ( 'NONE', #18407 ) ;
#2208 = CARTESIAN_POINT ( 'NONE',  ( -80.90000000000000568, -34.35000000000000853, -97.40192378864668399 ) ) ;
#2209 = CARTESIAN_POINT ( 'NONE',  ( 232.5999999999999375, -34.55624999877095860, -53.00000000000011369 ) ) ;
#2210 = CARTESIAN_POINT ( 'NONE',  ( 231.3931070460713499, -35.00000000000000000, -52.75353082432724960 ) ) ;
#2211 = CARTESIAN_POINT ( 'NONE',  ( -82.39999999999999147, -35.09062499938548285, -96.81714838363319586 ) ) ;
#2212 = CARTESIAN_POINT ( 'NONE',  ( 229.8435696437499303, -32.39062499938548001, 99.99999999999998579 ) ) ;
#2213 = CARTESIAN_POINT ( 'NONE',  ( -83.90000000000000568, -35.27268749875867826, 102.5980762113533018 ) ) ;
#2214 =( REPRESENTATION_RELATIONSHIP ('NONE','NONE', #14468, #16991 ) REPRESENTATION_RELATIONSHIP_WITH_TRANSFORMATION ( #8659 )SHAPE_REPRESENTATION_RELATIONSHIP( ) );
#2215 = CARTESIAN_POINT ( 'NONE',  ( -79.64356964375001269, -35.01562499938548711, 101.5914258081833879 ) ) ;
#2216 = LINE ( 'NONE', #15507, #18193 ) ;
#2217 = CARTESIAN_POINT ( 'NONE',  ( -85.40000000000000568, -33.05624999877097281, -98.26794919243111792 ) ) ;
#2218 = CARTESIAN_POINT ( 'NONE',  ( 82.39999999999999147, -31.49062499938548854, -103.1828516163667899 ) ) ;
#2219 = CARTESIAN_POINT ( 'NONE',  ( 80.90000000000000568, -34.64999999999999858, 102.5980762113533018 ) ) ;
#2220 = ORIENTED_EDGE ( 'NONE', *, *, #14527, .T. ) ;
#2221 = CARTESIAN_POINT ( 'NONE',  ( 231.2217848218749339, -34.67812499938548143, -47.61286128772501769 ) ) ;
#2222 = CONTEXT_DEPENDENT_SHAPE_REPRESENTATION ( #8212, #2335 ) ;
#2223 = CARTESIAN_POINT ( 'NONE',  ( 233.9782151781249411, -33.55312499938548143, 97.61286128772489690 ) ) ;
#2224 = CARTESIAN_POINT ( 'NONE',  ( 235.3564303562499447, -34.04062499938547859, -51.59142580818350865 ) ) ;
#2225 = B_SPLINE_CURVE_WITH_KNOTS ( 'NONE', 3,
 ( #19, #17794, #16324, #5873, #11825, #2837, #7425, #8791, #2933, #14749, #8886, #1382, #14949, #14845, #1470, #13385 ),
 .UNSPECIFIED., .F., .F.,
 ( 4, 2, 2, 2, 2, 2, 2, 4 ),
 ( 0.000000000000000000, 0.0005391024520904520593, 0.001078204904180904119, 0.002156409808361781782, 0.002695512260452248912, 0.003234614712542715608, 0.003773717164633182304, 0.004312819616723649434 ),
 .UNSPECIFIED. ) ;
#2226 = CARTESIAN_POINT ( 'NONE',  ( -82.39999999999999147, -32.50312499938548427, 96.81714838363319586 ) ) ;
#2227 = CARTESIAN_POINT ( 'NONE',  ( -84.75088379146902184, -34.99999999999999289, -98.39201219457972059 ) ) ;
#2228 = ORIENTED_EDGE ( 'NONE', *, *, #6672, .F. ) ;
#2230 = EDGE_LOOP ( 'NONE', ( #5939, #17615, #6763 ) ) ;
#2229 = EDGE_CURVE ( 'NONE', #4020, #14453, #5179, .T. ) ;
#2231 = CARTESIAN_POINT ( 'NONE',  ( -83.77821517812500929, -30.66562499938548569, -102.3871387122750889 ) ) ;
#2232 = ORIENTED_EDGE ( 'NONE', *, *, #8150, .T. ) ;
#2233 = CARTESIAN_POINT ( 'NONE',  ( 79.64356964374999848, -33.17812499938548854, 99.99999999999998579 ) ) ;
#2234 = CARTESIAN_POINT ( 'NONE',  ( -82.39999999999999147, -33.43124999877097281, -96.53589838486223584 ) ) ;
#2235 = CARTESIAN_POINT ( 'NONE',  ( 232.5999999999999375, -33.20624999877097139, -53.00000000000011369 ) ) ;
#2236 = DIRECTION ( 'NONE',  ( 0.000000000000000000, -1.000000000000000000, 0.000000000000000000 ) ) ;
#2237 = CARTESIAN_POINT ( 'NONE',  ( -82.39999999999999147, -33.20624999877097139, 96.53589838486223584 ) ) ;
#2238 = CARTESIAN_POINT ( 'NONE',  ( -80.90000000000000568, -34.29374999877096997, 102.5980762113533018 ) ) ;
#2239 = FACE_OUTER_BOUND ( 'NONE', #2585, .T. ) ;
#2240 = DIRECTION ( 'NONE',  ( 1.000000000000000000, -1.387778780781445676E-15, -2.407412430484046130E-31 ) ) ;
#2241 = CARTESIAN_POINT ( 'NONE',  ( -80.90000000000000568, -34.14374999877097139, 97.40192378864668399 ) ) ;
#2242 = CARTESIAN_POINT ( 'NONE',  ( 231.2217848218749339, -33.66562499938547859, 102.3871387122750889 ) ) ;
#2243 = ORIENTED_EDGE ( 'NONE', *, *, #6057, .T. ) ;
#2244 = EDGE_CURVE ( 'NONE', #5317, #1228, #1301, .T. ) ;
#2245 = CARTESIAN_POINT ( 'NONE',  ( 81.02178482187500208, -33.59062499938548285, -102.3871387122750889 ) ) ;
#2246 = CARTESIAN_POINT ( 'NONE',  ( 235.5999999999999943, -31.55624999877096215, 101.7320508075688537 ) ) ;
#2247 = DIRECTION ( 'NONE',  ( 0.000000000000000000, 0.000000000000000000, 1.000000000000000000 ) ) ;
#2248 = ORIENTED_EDGE ( 'NONE', *, *, #14234, .F. ) ;
#2249 = CARTESIAN_POINT ( 'NONE',  ( 229.5999999999999375, -34.46249999999999147, 101.7320508075688821 ) ) ;
#2250 = CARTESIAN_POINT ( 'NONE',  ( 1.317756351988342622, -3.857995168970215438, -0.04852650426602527628 ) ) ;
#2251 = DIRECTION ( 'NONE',  ( -0.000000000000000000, -0.000000000000000000, 1.000000000000000000 ) ) ;
#2252 = ORIENTED_EDGE ( 'NONE', *, *, #175, .F. ) ;
#2253 = CARTESIAN_POINT ( 'NONE',  ( 96.99999999999994316, -21.80000000000003268, -139.9999999999999716 ) ) ;
#2254 = AXIS2_PLACEMENT_3D ( 'NONE', #5055, #18531, #14119 ) ;
#2255 = CARTESIAN_POINT ( 'NONE',  ( -79.39999999999999147, -33.73124999877096997, 98.26794919243110371 ) ) ;
#2256 = VERTEX_POINT ( 'NONE', #12439 ) ;
#2257 = SURFACE_SIDE_STYLE ('',( #18875 ) ) ;
#2258 = CARTESIAN_POINT ( 'NONE',  ( 79.39999999999999147, -32.51250000000000284, -101.7320508075688537 ) ) ;
#2259 = DIRECTION ( 'NONE',  ( -1.000000000000000000, 0.000000000000000000, 0.000000000000000000 ) ) ;
#2260 = CARTESIAN_POINT ( 'NONE',  ( -85.40000000000000568, -33.99374999877097281, 99.99999999999998579 ) ) ;
#2261 = CARTESIAN_POINT ( 'NONE',  ( -79.39999999999999147, -34.75856250001229597, 101.7320508075688537 ) ) ;
#2262 = CARTESIAN_POINT ( 'NONE',  ( -2.499999999999999556, 3.061616997868382648E-16, 3.469446951953614189E-15 ) ) ;
#2263 = CARTESIAN_POINT ( 'NONE',  ( 229.5999999999999375, -33.18749999999999289, 98.26794919243111792 ) ) ;
#2264 = CARTESIAN_POINT ( 'NONE',  ( 229.5999999999999375, -32.23124999877096286, -51.73205080756898866 ) ) ;
#2265 = EDGE_CURVE ( 'NONE', #711, #15407, #14092, .T. ) ;
#2266 = CARTESIAN_POINT ( 'NONE',  ( 246.9999999999999716, -5.000000000000004441, -100.0000000000000000 ) ) ;
#2267 = CARTESIAN_POINT ( 'NONE',  ( -85.15643035624999868, -32.87812499938549138, 98.40857419181659793 ) ) ;
#2268 = PRESENTATION_LAYER_ASSIGNMENT (  '', '', ( #5710 ) ) ;
#2269 =( BOUNDED_CURVE ( )  B_SPLINE_CURVE ( 2, ( #115, #7422, #13382, #16414, #1663, #16, #4494 ),
 .UNSPECIFIED., .F., .F. ) 
 B_SPLINE_CURVE_WITH_KNOTS ( ( 3, 2, 2, 3 ),
 ( 0.8958333333333333703, 0.9027777777777777901, 0.9166666666666666297, 0.9258785066912882389 ),
 .UNSPECIFIED. ) 
 CURVE ( )  GEOMETRIC_REPRESENTATION_ITEM ( )  RATIONAL_B_SPLINE_CURVE ( ( 0.9330127018922192983, 0.9330127018922198534, 1.000000000000000000, 0.8660254037844387076, 1.000000000000000000, 0.9111410165655264848, 0.9401539157124900736 ) ) 
 REPRESENTATION_ITEM ( '' )  );
#2270 = AXIS2_PLACEMENT_3D ( 'NONE', #18762, #2049, #11233 ) ;
#2271 = CARTESIAN_POINT ( 'NONE',  ( 84.51154815724953551, -35.14114861271051637, -98.22820072003833047 ) ) ;
#2272 = ORIENTED_EDGE ( 'NONE', *, *, #12971, .F. ) ;
#2273 = CARTESIAN_POINT ( 'NONE',  ( 232.5999999999999375, -29.99999999999999645, 96.99999999999998579 ) ) ;
#2274 = CARTESIAN_POINT ( 'NONE',  ( -79.39999999999999147, -34.27499999999999858, 99.99999999999998579 ) ) ;
#2275 = FACE_OUTER_BOUND ( 'NONE', #5001, .T. ) ;
#2276 = CARTESIAN_POINT ( 'NONE',  ( 231.0999999999999375, -34.87499999999999289, -47.40192378864679768 ) ) ;
#2277 = CARTESIAN_POINT ( 'NONE',  ( -81.02178482187500208, -34.90312499938548285, 97.61286128772489690 ) ) ;
#2278 = CARTESIAN_POINT ( 'NONE',  ( 235.3564303562499447, -35.01562499938548001, -48.40857419181671162 ) ) ;
#2279 = EDGE_LOOP ( 'NONE', ( #4183, #10015, #9450, #7227 ) ) ;
#2280 = CARTESIAN_POINT ( 'NONE',  ( 4.052432342741377980, 1.393590342654233316, 3.567979436357326062 ) ) ;
#2281 = AXIS2_PLACEMENT_3D ( 'NONE', #15257, #6282, #6184 ) ;
#2282 = CARTESIAN_POINT ( 'NONE',  ( 4.175813232069147674, 2.061359961916367833, 3.570380186727398097 ) ) ;
#2283 = CARTESIAN_POINT ( 'NONE',  ( 79.64356964375001269, -33.47812499938547859, 101.5914258081833879 ) ) ;
#2284 = CARTESIAN_POINT ( 'NONE',  ( -2.742827927723112236, -3.035229711105190464, -3.433252694550595230 ) ) ;
#2285 = CARTESIAN_POINT ( 'NONE',  ( 230.7186334667984227, -32.00000000000000711, -52.01453922190813728 ) ) ;
#2286 = CARTESIAN_POINT ( 'NONE',  ( -83.77821517812500929, -32.87812499938548427, 102.3871387122750889 ) ) ;
#2287 = DIRECTION ( 'NONE',  ( -0.000000000000000000, -0.000000000000000000, -1.000000000000000000 ) ) ;
#2288 = CARTESIAN_POINT ( 'NONE',  ( 82.39999999999999147, -32.50312499938548427, 103.1828516163667899 ) ) ;
#2289 = CARTESIAN_POINT ( 'NONE',  ( 85.15643035625001289, -34.75312499938548427, -99.99999999999998579 ) ) ;
#2290 = CARTESIAN_POINT ( 'NONE',  ( 231.2217848218749339, -32.76562499938548001, -47.61286128772501769 ) ) ;
#2291 = CARTESIAN_POINT ( 'NONE',  ( -81.02178482187500208, -33.25312499938548427, 102.3871387122750889 ) ) ;
#2292 = VERTEX_POINT ( 'NONE', #5027 ) ;
#2293 = CARTESIAN_POINT ( 'NONE',  ( 85.15643035624999868, -32.54062499938548569, 101.5914258081833879 ) ) ;
#2294 = CARTESIAN_POINT ( 'NONE',  ( -79.39999999999999147, -33.82500000000000284, 99.99999999999998579 ) ) ;
#2295 = ADVANCED_FACE ( 'NONE', ( #6391 ), #2718, .T. ) ;
#2296 = CARTESIAN_POINT ( 'NONE',  ( -82.39999999999999147, -30.47812499938548569, 103.1828516163667899 ) ) ;
#2297 = CARTESIAN_POINT ( 'NONE',  ( -82.39999999999999147, -33.29062499938549280, 103.1828516163667899 ) ) ;
#2298 = FACE_OUTER_BOUND ( 'NONE', #2561, .T. ) ;
#2299 = VERTEX_POINT ( 'NONE', #11065 ) ;
#2300 = CARTESIAN_POINT ( 'NONE',  ( -83.90000000000000568, -32.62500000000000000, -97.40192378864668399 ) ) ;
#2301 = CARTESIAN_POINT ( 'NONE',  ( 1.747541505913279281, -3.837784562140273081, -3.503702292528912299 ) ) ;
#2302 = DIRECTION ( 'NONE',  ( -0.000000000000000000, -1.000000000000000000, -0.000000000000000000 ) ) ;
#2303 = CARTESIAN_POINT ( 'NONE',  ( -79.39999999999999147, -30.70856250001229526, 101.7320508075688537 ) ) ;
#2304 = EDGE_CURVE ( 'NONE', #4985, #13752, #9705, .T. ) ;
#2305 = CARTESIAN_POINT ( 'NONE',  ( -85.40000000000000568, -33.58518749875867826, 98.26794919243111792 ) ) ;
#2306 = CARTESIAN_POINT ( 'NONE',  ( -82.40000000000001990, -32.75624999877096855, 97.00000000000000000 ) ) ;
#2307 = CARTESIAN_POINT ( 'NONE',  ( 235.5999999999999943, -32.88749999999999574, 98.26794919243110371 ) ) ;
#2308 = CARTESIAN_POINT ( 'NONE',  ( 79.64356964374998427, -34.90312499938548285, 98.40857419181659793 ) ) ;
#2309 = CARTESIAN_POINT ( 'NONE',  ( 81.02178482187500208, -30.55312499938548854, 97.61286128772489690 ) ) ;
#2310 = FACE_OUTER_BOUND ( 'NONE', #8168, .T. ) ;
#2311 = CARTESIAN_POINT ( 'NONE',  ( 232.3466685930879123, -34.99995246259152282, -52.98928446312130802 ) ) ;
#2312 = CARTESIAN_POINT ( 'NONE',  ( 83.77821517812500929, -32.12812499938548427, -97.61286128772489690 ) ) ;
#2313 = CARTESIAN_POINT ( 'NONE',  ( -83.20384757729333103, -33.18615380933863435, 96.99999999999997158 ) ) ;
#2314 = ORIENTED_EDGE ( 'NONE', *, *, #16158, .T. ) ;
#2315 = CARTESIAN_POINT ( 'NONE',  ( 85.40000000000000568, -30.39374999877097139, 99.99999999999998579 ) ) ;
#2316 = APPLICATION_PROTOCOL_DEFINITION ( 'draft international standard', 'automotive_design', 1998, #11203 ) ;
#2317 = ADVANCED_FACE ( 'NONE', ( #2275 ), #18527, .F. ) ;
#2318 = CARTESIAN_POINT ( 'NONE',  ( 229.8435696437499871, -34.79062499938547859, 98.40857419181659793 ) ) ;
#2319 = CARTESIAN_POINT ( 'NONE',  ( 229.8435696437499303, -33.85312499938548569, -50.00000000000011369 ) ) ;
#2320 = EDGE_CURVE ( 'NONE', #17568, #9852, #15512, .T. ) ;
#2321 = CARTESIAN_POINT ( 'NONE',  ( -81.02178482187500208, -33.59062499938548285, 102.3871387122750889 ) ) ;
#2322 = CARTESIAN_POINT ( 'NONE',  ( 83.90000000000000568, -33.97500000000000853, 97.40192378864668399 ) ) ;
#2323 = ORIENTED_EDGE ( 'NONE', *, *, #16523, .F. ) ;
#2324 = CARTESIAN_POINT ( 'NONE',  ( -81.02178482187500208, -32.69062499938548427, -97.61286128772489690 ) ) ;
#2325 = EDGE_CURVE ( 'NONE', #17759, #5681, #5512, .T. ) ;
#2326 = DIRECTION ( 'NONE',  ( 1.000000000000000000, -1.577021341797101948E-15, 0.000000000000000000 ) ) ;
#2327 = VERTEX_POINT ( 'NONE', #11554 ) ;
#2328 = CARTESIAN_POINT ( 'NONE',  ( 79.64356964374998427, -34.04062499938549280, 101.5914258081833879 ) ) ;
#2329 = CARTESIAN_POINT ( 'NONE',  ( -85.40000000000000568, -35.30624999877096570, -98.26794919243111792 ) ) ;
#2330 = CARTESIAN_POINT ( 'NONE',  ( 79.39999999999999147, -33.86250000000000426, 98.26794919243113213 ) ) ;
#2331 = CARTESIAN_POINT ( 'NONE',  ( 233.9782151781249411, -30.40312499938547930, 97.61286128772489690 ) ) ;
#2332 = CARTESIAN_POINT ( 'NONE',  ( -79.39999999999999147, -33.35624999877097707, 101.7320508075688537 ) ) ;
#2333 = CARTESIAN_POINT ( 'NONE',  ( -81.02178482187500208, -31.00312499938548783, 102.3871387122750889 ) ) ;
#2334 = CARTESIAN_POINT ( 'NONE',  ( -82.40000000000000568, -30.73124999877097352, 102.9999999999999858 ) ) ;
#2335 = PRODUCT_DEFINITION_SHAPE ( 'NONE', 'NONE',  #19322 ) ;
#2336 = PLANE ( 'NONE',  #16751 ) ;
#2337 = ADVANCED_FACE ( 'NONE', ( #17324 ), #13017, .F. ) ;
#2338 = DIRECTION ( 'NONE',  ( -0.000000000000000000, -0.000000000000000000, -1.000000000000000000 ) ) ;
#2339 = CARTESIAN_POINT ( 'NONE',  ( 231.0999999999999375, -32.32499999999999574, 97.40192378864668399 ) ) ;
#2340 = ORIENTED_EDGE ( 'NONE', *, *, #18683, .F. ) ;
#2341 = CARTESIAN_POINT ( 'NONE',  ( 82.39999999999999147, -32.72812499938548569, -103.1828516163667899 ) ) ;
#2342 =( LENGTH_UNIT ( ) NAMED_UNIT ( * ) SI_UNIT ( .MILLI., .METRE. ) );
#2343 = CARTESIAN_POINT ( 'NONE',  ( 231.0999999999999375, -30.46874999877096002, 97.40192378864668399 ) ) ;
#2344 = CARTESIAN_POINT ( 'NONE',  ( 235.5999999999999943, -31.93124999877096570, -51.73205080756900287 ) ) ;
#2345 = ORIENTED_EDGE ( 'NONE', *, *, #2657, .F. ) ;
#2346 = CARTESIAN_POINT ( 'NONE',  ( 85.40000000000000568, -32.70000000000000284, 99.99999999999998579 ) ) ;
#2347 = CARTESIAN_POINT ( 'NONE',  ( -85.15643035625001289, -30.62812499938548427, 98.40857419181659793 ) ) ;
#2348 = ORIENTED_EDGE ( 'NONE', *, *, #12952, .T. ) ;
#2349 = CARTESIAN_POINT ( 'NONE',  ( -81.59615242270662350, -32.06115380933863435, 103.0000000000000000 ) ) ;
#2350 = CIRCLE ( 'NONE', #12947, 2.199999999999993516 ) ;
#2351 = DIRECTION ( 'NONE',  ( 1.000000000000000000, 0.000000000000000000, 4.163336342344333240E-14 ) ) ;
#2352 = ORIENTED_EDGE ( 'NONE', *, *, #10186, .F. ) ;
#2353 = CARTESIAN_POINT ( 'NONE',  ( 79.39999999999999147, -33.82500000000000284, -99.99999999999998579 ) ) ;
#2354 = EDGE_CURVE ( 'NONE', #15766, #19154, #11162, .T. ) ;
#2355 = CARTESIAN_POINT ( 'NONE',  ( 82.40000000000000568, -30.00000000000000355, -99.99999999999998579 ) ) ;
#2356 = CARTESIAN_POINT ( 'NONE',  ( -83.77821517812500929, -31.52812499938548996, 102.3871387122750889 ) ) ;
#2357 = CARTESIAN_POINT ( 'NONE',  ( -79.39999999999999147, -30.18750000000000355, 98.26794919243110371 ) ) ;
#2358 = CARTESIAN_POINT ( 'NONE',  ( -81.59615242270662350, -33.41115380933863577, 102.9999999999999858 ) ) ;
#2359 = CARTESIAN_POINT ( 'NONE',  ( 0.1397371499203162448, 1.362866705341262641, -3.500000000000000444 ) ) ;
#2360 = CARTESIAN_POINT ( 'NONE',  ( 83.20384757729335945, -33.90134618820329848, 96.99999999999998579 ) ) ;
#2361 = EDGE_CURVE ( 'NONE', #15766, #19060, #5321, .T. ) ;
#2362 = CYLINDRICAL_SURFACE ( 'NONE', #4018, 6.000000000000005329 ) ;
#2363 = CARTESIAN_POINT ( 'NONE',  ( -85.15643035624999868, -32.80312499938548854, 101.5914258081833879 ) ) ;
#2364 = VECTOR ( 'NONE', #12931, 1000.000000000000000 ) ;
#2365 = CARTESIAN_POINT ( 'NONE',  ( 82.40000000000000568, -30.00000000000000355, 96.99999999999998579 ) ) ;
#2366 = ORIENTED_EDGE ( 'NONE', *, *, #2123, .F. ) ;
#2367 = CARTESIAN_POINT ( 'NONE',  ( 232.5999999999999375, -34.16249999999999432, -53.46410161513786363 ) ) ;
#2368 = CARTESIAN_POINT ( 'NONE',  ( -82.40000000000001990, -33.20624999877097849, 97.00000000000000000 ) ) ;
#2370 = FACE_OUTER_BOUND ( 'NONE', #17466, .T. ) ;
#2369 = B_SPLINE_CURVE_WITH_KNOTS ( 'NONE', 3,
 ( #14521, #8285, #14236, #1154, #7113, #18750, #2227, #2422, #8382, #971, #12874, #11885, #1253, #17662, #9050, #7588, #10139, #6036 ),
 .UNSPECIFIED., .F., .F.,
 ( 4, 2, 2, 2, 2, 2, 2, 2, 4 ),
 ( 0.000000000000000000, 0.0007089252359836130824, 0.001417850471967226165, 0.002126775707950839464, 0.002835700943934452330, 0.003544626179918065195, 0.004253551415901678928, 0.004962476651885291794, 0.005671401887868904659 ),
 .UNSPECIFIED. ) ;
#2371 = CARTESIAN_POINT ( 'NONE',  ( -79.64356964375001269, -34.56562499938549138, 101.5914258081833879 ) ) ;
#2372 = CARTESIAN_POINT ( 'NONE',  ( 233.9782151781249411, -34.60312499938548569, -47.61286128772501769 ) ) ;
#2373 = AXIS2_PLACEMENT_3D ( 'NONE', #9068, #12296, #13558 ) ;
#2374 = VERTEX_POINT ( 'NONE', #17426 ) ;
#2375 = CARTESIAN_POINT ( 'NONE',  ( -82.85452780460290967, -35.00000000000000000, -97.27546421900275675 ) ) ;
#2376 = CARTESIAN_POINT ( 'NONE',  ( -82.39999999999999147, -34.52812499938548996, 103.1828516163667899 ) ) ;
#2377 = AXIS2_PLACEMENT_3D ( 'NONE', #15410, #11206, #17171 ) ;
#2378 = CARTESIAN_POINT ( 'NONE',  ( 111.5000000000000142, 12.69999999999998508, 50.00000000000001421 ) ) ;
#2379 = CARTESIAN_POINT ( 'NONE',  ( 83.77821517812500929, -33.66562499938548569, 97.61286128772489690 ) ) ;
#2380 = CARTESIAN_POINT ( 'NONE',  ( 0.1410422978106145031, -4.700232962125109104, -3.687027686973628704 ) ) ;
#2381 = CARTESIAN_POINT ( 'NONE',  ( 110.0000000000000000, 10.19999999999997620, -139.9999999999999716 ) ) ;
#2382 = CARTESIAN_POINT ( 'NONE',  ( -85.15643035625001289, -34.26562499938548711, 101.5914258081833879 ) ) ;
#2383 = CARTESIAN_POINT ( 'NONE',  ( -83.77821517812500929, -33.77812499938548285, -97.61286128772489690 ) ) ;
#2384 = CARTESIAN_POINT ( 'NONE',  ( 85.15643035625001289, -31.94062499938548427, 99.99999999999998579 ) ) ;
#2385 = CARTESIAN_POINT ( 'NONE',  ( -81.22643902596118437, -32.00000000000000000, -102.6636594982756492 ) ) ;
#2386 = CARTESIAN_POINT ( 'NONE',  ( 85.15643035625001289, -33.85312499938549280, -99.99999999999998579 ) ) ;
#2387 = CARTESIAN_POINT ( 'NONE',  ( 231.2217848218749339, -32.91562499938547148, -52.38713871227520968 ) ) ;
#2388 = CARTESIAN_POINT ( 'NONE',  ( -79.64356964374998427, -33.10312499938548569, 101.5914258081833879 ) ) ;
#2389 = CARTESIAN_POINT ( 'NONE',  ( 81.02178482187500208, -30.74062499938548498, -97.61286128772489690 ) ) ;
#2390 = ORIENTED_EDGE ( 'NONE', *, *, #9593, .F. ) ;
#2391 = DIRECTION ( 'NONE',  ( 0.000000000000000000, 0.000000000000000000, 1.000000000000000000 ) ) ;
#2392 = LINE ( 'NONE', #4154, #11487 ) ;
#2393 = CARTESIAN_POINT ( 'NONE',  ( -80.90000000000000568, -32.40000000000000568, 97.40192378864668399 ) ) ;
#2394 = CARTESIAN_POINT ( 'NONE',  ( -81.02178482187500208, -31.34062499938548996, 102.3871387122750889 ) ) ;
#2395 = CARTESIAN_POINT ( 'NONE',  ( -81.02178482187500208, -30.74062499938548498, 97.61286128772489690 ) ) ;
#2396 = CARTESIAN_POINT ( 'NONE',  ( 246.9999999999999716, -29.80000000000000426, -100.0000000000000000 ) ) ;
#2397 = ORIENTED_EDGE ( 'NONE', *, *, #10186, .T. ) ;
#2398 = CARTESIAN_POINT ( 'NONE',  ( -80.90000000000000568, -34.64999999999999858, -102.5980762113533018 ) ) ;
#2399 = CARTESIAN_POINT ( 'NONE',  ( 79.39999999999999147, -32.88750000000000284, -98.26794919243110371 ) ) ;
#2400 = FACE_BOUND ( 'NONE', #4345, .T. ) ;
#2401 = CARTESIAN_POINT ( 'NONE',  ( 81.59615242270662350, -32.06115380933863435, -103.0000000000000000 ) ) ;
#2402 = VECTOR ( 'NONE', #3776, 1000.000000000000000 ) ;
#2403 = FACE_OUTER_BOUND ( 'NONE', #17857, .T. ) ;
#2404 = CARTESIAN_POINT ( 'NONE',  ( -81.02178482187500208, -30.44062499938548783, 102.3871387122750889 ) ) ;
#2405 = CARTESIAN_POINT ( 'NONE',  ( -81.59615242270663771, -32.51115380933863008, -96.99999999999998579 ) ) ;
#2406 = CARTESIAN_POINT ( 'NONE',  ( 79.64356964375001269, -30.89062499938548711, 101.5914258081833879 ) ) ;
#2407 = CARTESIAN_POINT ( 'NONE',  ( 231.4797793666089945, -32.00000000000000711, 97.42682425340032637 ) ) ;
#2408 = AXIS2_PLACEMENT_3D ( 'NONE', #5217, #10778, #15666 ) ;
#2409 = DIRECTION ( 'NONE',  ( 1.387778780781445676E-15, 1.000000000000000000, 0.000000000000000000 ) ) ;
#2410 = CARTESIAN_POINT ( 'NONE',  ( 85.15643035625001289, -34.75312499938548427, -99.99999999999998579 ) ) ;
#2411 = CYLINDRICAL_SURFACE ( 'NONE', #16456, 10.00000000000000000 ) ;
#2412 = EDGE_LOOP ( 'NONE', ( #1035, #4107, #3673, #1185 ) ) ;
#2413 = CARTESIAN_POINT ( 'NONE',  ( 79.39999999999999147, -31.10624999877097352, 98.26794919243113213 ) ) ;
#2414 = ITEM_DEFINED_TRANSFORMATION ( 'NONE', 'NONE', #11430,  #10540 ) ;
#2415 = CARTESIAN_POINT ( 'NONE',  ( 229.8435696437499303, -33.85312499938548569, 99.99999999999998579 ) ) ;
#2416 = CARTESIAN_POINT ( 'NONE',  ( 233.9782151781249411, -32.20312499938548001, -52.38713871227520968 ) ) ;
#2417 = CIRCLE ( 'NONE', #4292, 4.000000000000000000 ) ;
#2418 = EDGE_CURVE ( 'NONE', #9387, #6061, #324, .T. ) ;
#2419 =( GEOMETRIC_REPRESENTATION_CONTEXT ( 3 ) GLOBAL_UNCERTAINTY_ASSIGNED_CONTEXT ( ( #18388 ) ) GLOBAL_UNIT_ASSIGNED_CONTEXT ( ( #5002, #1864, #15640 ) ) REPRESENTATION_CONTEXT ( 'NONE', 'WORKASPACE' ) );
#2420 = EDGE_CURVE ( 'NONE', #15931, #19033, #10026, .T. ) ;
#2421 = CARTESIAN_POINT ( 'NONE',  ( 233.4038475772933054, -34.12634618820329280, 96.99999999999997158 ) ) ;
#2422 = CARTESIAN_POINT ( 'NONE',  ( -85.00132729414812616, -34.99999999999999289, -98.78874432549871187 ) ) ;
#2423 = ORIENTED_EDGE ( 'NONE', *, *, #9224, .F. ) ;
#2424 = CARTESIAN_POINT ( 'NONE',  ( -83.77821517812500929, -31.41562499938548569, -97.61286128772489690 ) ) ;
#2425 = CARTESIAN_POINT ( 'NONE',  ( 82.40000000000000568, -32.30624999877097281, 102.9999999999999858 ) ) ;
#2426 = ORIENTED_EDGE ( 'NONE', *, *, #3306, .F. ) ;
#2427 = CARTESIAN_POINT ( 'NONE',  ( 82.39999999999999147, -33.74062499938548854, 96.81714838363319586 ) ) ;
#2428 = VECTOR ( 'NONE', #12896, 1000.000000000000000 ) ;
#2429 = CARTESIAN_POINT ( 'NONE',  ( -81.02178482187500208, -31.90312499938548996, -97.61286128772489690 ) ) ;
#2430 = CARTESIAN_POINT ( 'NONE',  ( -85.40000000000000568, -30.39374999877097139, -99.99999999999998579 ) ) ;
#2431 = CARTESIAN_POINT ( 'NONE',  ( 82.40000000000000568, -34.78124999877096712, -102.9999999999999858 ) ) ;
#2432 = CARTESIAN_POINT ( 'NONE',  ( -80.90000000000000568, -33.39374999877097139, 102.5980762113533018 ) ) ;
#2433 = CARTESIAN_POINT ( 'NONE',  ( -79.64356964375001269, -32.24062499938548854, 98.40857419181659793 ) ) ;
#2434 = CIRCLE ( 'NONE', #8986, 5.199999999999996625 ) ;
#2435 = CARTESIAN_POINT ( 'NONE',  ( -82.39999999999999147, -32.72812499938548569, -96.81714838363319586 ) ) ;
#2436 = CIRCLE ( 'NONE', #17096, 7.500000000000020428 ) ;
#2437 = EDGE_CURVE ( 'NONE', #12229, #729, #922, .T. ) ;
#2438 = CARTESIAN_POINT ( 'NONE',  ( 231.7961524227065695, -32.34240381056765301, -53.00000000000011369 ) ) ;
#2439 = ADVANCED_FACE ( 'NONE', ( #19078 ), #6879, .F. ) ;
#2440 = CARTESIAN_POINT ( 'NONE',  ( 235.0681666926251694, -31.99999999999997158, 101.6855250459193627 ) ) ;
#2441 = CARTESIAN_POINT ( 'NONE',  ( 229.5999999999999375, -29.99999999999999645, 99.99999999999998579 ) ) ;
#2442 = EDGE_LOOP ( 'NONE', ( #18, #13707, #1278 ) ) ;
#2443 = CARTESIAN_POINT ( 'NONE',  ( 85.15643035625001289, -33.29062499938547859, -99.99999999999998579 ) ) ;
#2444 = FILL_AREA_STYLE_COLOUR ( '', #12359 ) ;
#2445 = CARTESIAN_POINT ( 'NONE',  ( 232.5999999999999375, -32.53124999877096002, 103.4641016151377499 ) ) ;
#2446 = CARTESIAN_POINT ( 'NONE',  ( 229.5999999999999375, -30.43124999877096215, -51.73205080756898866 ) ) ;
#2447 = VERTEX_POINT ( 'NONE', #11359 ) ;
#2448 = CARTESIAN_POINT ( 'NONE',  ( -79.39999999999999147, -35.11874999877096570, 99.99999999999998579 ) ) ;
#2449 = CARTESIAN_POINT ( 'NONE',  ( -82.39999999999999147, -30.70312499938548711, 96.81714838363319586 ) ) ;
#2450 = CARTESIAN_POINT ( 'NONE',  ( 4.071447262713888016, 4.041451884327382338, 0.000000000000000000 ) ) ;
#2451 = ORIENTED_EDGE ( 'NONE', *, *, #12261, .F. ) ;
#2452 = CARTESIAN_POINT ( 'NONE',  ( 232.5999999999999375, -33.65624999877096002, 97.00000000000000000 ) ) ;
#2453 = VECTOR ( 'NONE', #673, 1000.000000000000000 ) ;
#2454 = CARTESIAN_POINT ( 'NONE',  ( -80.90000000000000568, -33.69374999877096855, 97.40192378864668399 ) ) ;
#2455 = ORIENTED_EDGE ( 'NONE', *, *, #5799, .T. ) ;
#2456 = CARTESIAN_POINT ( 'NONE',  ( 82.39999999999999147, -33.26250000000000284, -96.53589838486223584 ) ) ;
#2457 = DIRECTION ( 'NONE',  ( -1.000000000000000000, -0.000000000000000000, -0.000000000000000000 ) ) ;
#2458 = CARTESIAN_POINT ( 'NONE',  ( -82.39999999999999147, -31.71562499938548640, 96.81714838363319586 ) ) ;
#2459 = CARTESIAN_POINT ( 'NONE',  ( -82.39999999999999147, -34.83356250001229171, 103.4641016151377499 ) ) ;
#2460 = CARTESIAN_POINT ( 'NONE',  ( 235.0804598586380507, -35.00000000000002132, -51.44276241308963193 ) ) ;
#2461 = CARTESIAN_POINT ( 'NONE',  ( 234.3965303555545461, -31.99999999999998579, -52.32517275847976634 ) ) ;
#2462 = CARTESIAN_POINT ( 'NONE',  ( 85.15643035625001289, -34.75312499938548427, -99.99999999999998579 ) ) ;
#2463 = CARTESIAN_POINT ( 'NONE',  ( -79.39999999999999147, -33.41250000000000142, 101.7320508075688537 ) ) ;
#2464 = CARTESIAN_POINT ( 'NONE',  ( 84.97511176747907768, -35.00000000000000000, 101.5169977320537669 ) ) ;
#2465 = CARTESIAN_POINT ( 'NONE',  ( -81.59615242270662350, -31.21740381056766722, 103.0000000000000000 ) ) ;
#2466 = VERTEX_POINT ( 'NONE', #3933 ) ;
#2467 = CARTESIAN_POINT ( 'NONE',  ( 233.4038475772933339, -32.06115380933863435, -47.00000000000011369 ) ) ;
#2468 = DIRECTION ( 'NONE',  ( -0.000000000000000000, -1.000000000000000000, -0.000000000000000000 ) ) ;
#2469 = CARTESIAN_POINT ( 'NONE',  ( 82.40000000000000568, -30.00000000000000355, 99.99999999999998579 ) ) ;
#2470 = CARTESIAN_POINT ( 'NONE',  ( 233.9782151781249411, -33.70312499938548001, 102.3871387122750889 ) ) ;
#2471 = CARTESIAN_POINT ( 'NONE',  ( -81.02178482187500208, -33.25312499938548427, 102.3871387122750889 ) ) ;
#2472 = CARTESIAN_POINT ( 'NONE',  ( 231.2217848218749339, -31.56562499938547717, -52.38713871227520968 ) ) ;
#2473 = ORIENTED_EDGE ( 'NONE', *, *, #6390, .T. ) ;
#2474 = EDGE_CURVE ( 'NONE', #17401, #13752, #15823, .T. ) ;
#2475 = CARTESIAN_POINT ( 'NONE',  ( -81.02178482187500208, -34.04062499938548569, 102.3871387122750889 ) ) ;
#2476 = DIRECTION ( 'NONE',  ( -7.222237291452147586E-32, 1.214306433183764966E-16, -1.000000000000000000 ) ) ;
#2477 = CARTESIAN_POINT ( 'NONE',  ( 80.90000000000000568, -30.75000000000000355, 97.40192378864668399 ) ) ;
#2478 = CARTESIAN_POINT ( 'NONE',  ( 83.90000000000000568, -32.71874999877096712, -97.40192378864668399 ) ) ;
#2479 = CARTESIAN_POINT ( 'NONE',  ( -82.39999999999999147, -34.86562499938548854, 96.81714838363319586 ) ) ;
#2480 = CARTESIAN_POINT ( 'NONE',  ( -81.02178482187500208, -34.45312499938548711, -102.3871387122750889 ) ) ;
#2481 = CARTESIAN_POINT ( 'NONE',  ( 83.77821517812500929, -32.76562499938548711, 97.61286128772489690 ) ) ;
#2482 = CARTESIAN_POINT ( 'NONE',  ( 83.77821517812500929, -34.37812499938548427, -97.61286128772489690 ) ) ;
#2483 = CARTESIAN_POINT ( 'NONE',  ( 232.5999999999999375, -33.62812499938547717, -46.81714838363331666 ) ) ;
#2484 = CARTESIAN_POINT ( 'NONE',  ( -81.02178482187500208, -33.14062499938548711, 102.3871387122750889 ) ) ;
#2485 = CARTESIAN_POINT ( 'NONE',  ( 82.39999999999999147, -31.15312499938548640, -96.81714838363319586 ) ) ;
#2486 = EDGE_LOOP ( 'NONE', ( #14026, #13933, #2455, #4660 ) ) ;
#2487 = CARTESIAN_POINT ( 'NONE',  ( 81.02178482187500208, -34.90312499938548285, 102.3871387122750889 ) ) ;
#2488 = ADVANCED_FACE ( 'NONE', ( #18102 ), #13331, .T. ) ;
#2489 = CARTESIAN_POINT ( 'NONE',  ( -85.15643035625001289, -30.14062499938548711, 99.99999999999998579 ) ) ;
#2490 = CARTESIAN_POINT ( 'NONE',  ( -85.40000000000000568, -32.66250000000000142, 101.7320508075688679 ) ) ;
#2491 = CARTESIAN_POINT ( 'NONE',  ( -83.77821517812500929, -33.36562499938548854, 97.61286128772489690 ) ) ;
#2492 = CARTESIAN_POINT ( 'NONE',  ( -82.39999999999999147, -31.37812499938548427, 103.1828516163667899 ) ) ;
#2493 = PRODUCT ( 'knife', 'knife', '', ( #12777 ) ) ;
#2494 = CARTESIAN_POINT ( 'NONE',  ( 232.5999999999999943, -32.05312499938548143, 96.81714838363319586 ) ) ;
#2495 = FACE_OUTER_BOUND ( 'NONE', #6682, .T. ) ;
#2496 = CARTESIAN_POINT ( 'NONE',  ( -79.39999999999999147, -31.08356250001229171, 98.26794919243110371 ) ) ;
#2497 = CARTESIAN_POINT ( 'NONE',  ( 4.158921614371307918, 1.986121848748763963, -3.559936047944504800 ) ) ;
#2498 = FACE_OUTER_BOUND ( 'NONE', #7291, .T. ) ;
#2499 = CARTESIAN_POINT ( 'NONE',  ( -81.02178482187500208, -30.74062499938548498, 97.61286128772489690 ) ) ;
#2500 = CARTESIAN_POINT ( 'NONE',  ( -80.90000000000000568, -32.49374999877097281, -97.40192378864668399 ) ) ;
#2501 = CARTESIAN_POINT ( 'NONE',  ( -82.40000000000001990, -34.61250000000001137, 97.00000000000000000 ) ) ;
#2502 = CARTESIAN_POINT ( 'NONE',  ( 235.3193635794330874, -31.99999999999998579, 98.73478688818596538 ) ) ;
#2503 = EDGE_CURVE ( 'NONE', #2622, #2968, #1394, .T. ) ;
#2504 = DIRECTION ( 'NONE',  ( -0.000000000000000000, 0.000000000000000000, -1.000000000000000000 ) ) ;
#2505 = CARTESIAN_POINT ( 'NONE',  ( 85.15643035624999868, -33.81562499938549138, -101.5914258081833879 ) ) ;
#2506 = CARTESIAN_POINT ( 'NONE',  ( -85.40000000000000568, -33.09374999877096712, 99.99999999999998579 ) ) ;
#2507 = VERTEX_POINT ( 'NONE', #10467 ) ;
#2508 = CARTESIAN_POINT ( 'NONE',  ( 80.90000000000000568, -33.24374999877097281, 102.5980762113533018 ) ) ;
#2509 = CARTESIAN_POINT ( 'NONE',  ( 233.5505106857032729, -35.00000000000002132, -47.40655328406458580 ) ) ;
#2510 = CARTESIAN_POINT ( 'NONE',  ( 229.8435696437499871, -32.09062499938548285, -51.59142580818350865 ) ) ;
#2511 = CARTESIAN_POINT ( 'NONE',  ( -81.02178482187500208, -34.94062499938548427, 102.3871387122750889 ) ) ;
#2512 = DIRECTION ( 'NONE',  ( -0.000000000000000000, 0.000000000000000000, -1.000000000000000000 ) ) ;
#2513 = ORIENTED_EDGE ( 'NONE', *, *, #4747, .F. ) ;
#2514 = CARTESIAN_POINT ( 'NONE',  ( -82.39999999999999147, -34.07812499938548711, -96.81714838363319586 ) ) ;
#2515 = DIRECTION ( 'NONE',  ( -0.000000000000000000, -1.000000000000000000, -0.000000000000000000 ) ) ;
#2516 = ORIENTED_EDGE ( 'NONE', *, *, #15618, .F. ) ;
#2517 = CARTESIAN_POINT ( 'NONE',  ( 85.15643035625001289, -34.26562499938548711, 98.40857419181659793 ) ) ;
#2518 = CARTESIAN_POINT ( 'NONE',  ( -83.90000000000000568, -35.26874999877097139, -97.40192378864668399 ) ) ;
#2519 = CARTESIAN_POINT ( 'NONE',  ( 83.90000000000000568, -33.52499999999999858, 97.40192378864668399 ) ) ;
#2520 = CARTESIAN_POINT ( 'NONE',  ( 246.9999999999999716, -5.000000000000004441, -100.0000000000000000 ) ) ;
#2521 = CARTESIAN_POINT ( 'NONE',  ( -84.69814161231455785, -35.39427329483935836, 98.07164704222793716 ) ) ;
#2522 = CARTESIAN_POINT ( 'NONE',  ( -79.64356964374999848, -31.37812499938548427, 99.99999999999998579 ) ) ;
#2523 = CARTESIAN_POINT ( 'NONE',  ( -83.77821517812500929, -33.66562499938548569, -97.61286128772489690 ) ) ;
#2524 = CYLINDRICAL_SURFACE ( 'NONE', #16136, 2.199999999999993516 ) ;
#2525 = CARTESIAN_POINT ( 'NONE',  ( 82.39999999999999147, -32.53124999877096712, -103.4641016151377499 ) ) ;
#2526 = CARTESIAN_POINT ( 'NONE',  ( 232.5999999999999375, -31.91249999999999432, 96.53589838486223584 ) ) ;
#2527 = ORIENTED_EDGE ( 'NONE', *, *, #2244, .F. ) ;
#2528 = CARTESIAN_POINT ( 'NONE',  ( 235.5999999999999943, -34.70624999877096428, 101.7320508075688537 ) ) ;
#2529 = CARTESIAN_POINT ( 'NONE',  ( 232.5999999999999375, -32.75624999877096144, 96.53589838486223584 ) ) ;
#2530 = CARTESIAN_POINT ( 'NONE',  ( 229.5999999999999375, -31.29374999877096286, -50.00000000000011369 ) ) ;
#2531 = CARTESIAN_POINT ( 'NONE',  ( 82.39999999999999147, -32.81250000000000000, 103.0000000000000000 ) ) ;
#2532 = CARTESIAN_POINT ( 'NONE',  ( -82.39999999999999147, -30.92812499938548143, 103.1828516163667899 ) ) ;
#2533 = ORIENTED_EDGE ( 'NONE', *, *, #6272, .F. ) ;
#2534 = ORIENTED_EDGE ( 'NONE', *, *, #15458, .F. ) ;
#2535 = CARTESIAN_POINT ( 'NONE',  ( 113.0000000000000000, 10.39615242270649276, -134.0032071715735640 ) ) ;
#2537 = EDGE_CURVE ( 'NONE', #12381, #5168, #9093, .T. ) ;
#2536 = CARTESIAN_POINT ( 'NONE',  ( 4.175326769692871309, -2.060699556488903017, 3.569236330973476257 ) ) ;
#2538 = ORIENTED_EDGE ( 'NONE', *, *, #16927, .T. ) ;
#2539 =( BOUNDED_CURVE ( )  B_SPLINE_CURVE ( 2, ( #460, #14205, #10795, #4850, #13817, #5341, #11476, #3854, #9918, #5528, #1119, #8731, #17535, #9817, #15880, #10111, #4246, #2577, #17443, #1220, #13035, #16066, #19096, #11279, #2672, #6896, #6986, #12751, #5717, #13126, #15779, #2388, #2484, #8631, #18720, #8442, #8350, #7079, #14589, #7176, #8538, #2778, #14304, #940, #17247, #5626, #12845, #15971, #3953, #14395, #5438, #14488, #4054, #10013, #18814, #1033, #12937, #11572, #18909, #19006, #10204, #17631, #11377, #4150, #11667, #17343, #16167, #842, #6805, #1697, #16356, #4640, #1412, #13321, #10304, #17824, #4532, #9116, #8829, #18119, #19195, #19297, #16648 ),
 .UNSPECIFIED., .F., .F. ) 
 B_SPLINE_CURVE_WITH_KNOTS ( ( 3, 2, 2, 2, 2, 2, 2, 2, 2, 2, 2, 2, 2, 2, 2, 2, 2, 2, 2, 2, 2, 2, 2, 2, 2, 2, 2, 2, 2, 2, 2, 2, 2, 2, 2, 2, 2, 2, 2, 2, 2, 3 ),
 ( 0.3716916592826016164, 0.3750191855951754416, 0.3900199530189824570, 0.4050207204427894725, 0.4200214878665964879, 0.4350222552904035034, 0.4500230227142105188, 0.4650237901380175343, 0.4800245575618244942, 0.4950253249856315096, 0.5100260924094385251, 0.5250268598332455960, 0.5400276272570525560, 0.5550283946808595159, 0.5700291621046665869, 0.5850299295284735468, 0.6000306969522806178, 0.6150314643760875777, 0.6300322317998947597, 0.6450329992237016086, 0.6600337666475086795, 0.6750345340713157505, 0.6900353014951225994, 0.7050360689189296703, 0.7200368363427366303, 0.7350376037665438123, 0.7500383711903506612, 0.7650391386141577321, 0.7800399060379648031, 0.7950406734617718740, 0.8100414408855788340, 0.8250422083093857939, 0.8400429757331928649, 0.8550437431569997138, 0.8700445105808067847, 0.8850452780046138557, 0.9000460454284208156, 0.9150468128522278866, 0.9300475802760349575, 0.9450483476998419174, 0.9600491151236488774, 0.9717223562348836774 ),
 .UNSPECIFIED. ) 
 CURVE ( )  GEOMETRIC_REPRESENTATION_ITEM ( )  RATIONAL_B_SPLINE_CURVE ( ( 0.9537471549767033707, 0.9702812541832881443, 1.000000000000000000, 0.8660254037844387076, 1.000000000000000000, 0.8660254037844387076, 1.000000000000000000, 0.8660254037844387076, 1.000000000000000000, 0.8660254037844387076, 1.000000000000000000, 0.8660254037844387076, 1.000000000000000000, 0.8660254037844387076, 1.000000000000000000, 0.8660254037844387076, 1.000000000000000000, 0.8660254037844387076, 1.000000000000000000, 0.8660254037844387076, 1.000000000000000000, 0.8660254037844387076, 1.000000000000000000, 0.8660254037844387076, 1.000000000000000000, 0.8660254037844387076, 1.000000000000000000, 0.8660254037844387076, 1.000000000000000000, 0.8660254037844387076, 1.000000000000000000, 0.8660254037844387076, 1.000000000000000000, 0.8660254037844387076, 1.000000000000000000, 0.8660254037844387076, 1.000000000000000000, 0.8660254037844387076, 1.000000000000000000, 0.8660254037844387076, 1.000000000000000000, 0.8660254037844387076, 1.000000000000000000, 0.8660254037844387076, 1.000000000000000000, 0.8660254037844387076, 1.000000000000000000, 0.8660254037844387076, 1.000000000000000000, 0.8660254037844387076, 1.000000000000000000, 0.8660254037844387076, 1.000000000000000000, 0.8660254037844387076, 1.000000000000000000, 0.8660254037844387076, 1.000000000000000000, 0.8660254037844387076, 1.000000000000000000, 0.8660254037844387076, 1.000000000000000000, 0.8660254037844387076, 1.000000000000000000, 0.8660254037844387076, 1.000000000000000000, 0.8660254037844387076, 1.000000000000000000, 0.8660254037844387076, 1.000000000000000000, 0.8660254037844387076, 1.000000000000000000, 0.8660254037844387076, 1.000000000000000000, 0.8660254037844387076, 1.000000000000000000, 0.8660254037844387076, 1.000000000000000000, 0.8660254037844387076, 1.000000000000000000, 0.8660254037844387076, 1.000000000000000000, 0.8957441496011365745, 0.9537471549767190249 ) ) 
 REPRESENTATION_ITEM ( '' )  );
#2540 = CARTESIAN_POINT ( 'NONE',  ( 79.39999999999999147, -32.88750000000000284, -98.26794919243110371 ) ) ;
#2541 = CARTESIAN_POINT ( 'NONE',  ( 83.09162395290297809, -32.00000000000000000, -102.7516965079135502 ) ) ;
#2542 = CARTESIAN_POINT ( 'NONE',  ( -83.77821517812500929, -31.67812499938548498, 97.61286128772489690 ) ) ;
#2543 = CARTESIAN_POINT ( 'NONE',  ( -80.90000000000000568, -32.10000000000000142, 102.5980762113533018 ) ) ;
#2544 = CARTESIAN_POINT ( 'NONE',  ( 2.000000000000008882, 3.464101615137749945, 0.000000000000000000 ) ) ;
#2545 = EDGE_CURVE ( 'NONE', #18744, #15781, #14514, .T. ) ;
#2546 = CARTESIAN_POINT ( 'NONE',  ( 231.7961524227065695, -32.28615380933862156, -53.00000000000011369 ) ) ;
#2547 = CARTESIAN_POINT ( 'NONE',  ( 79.73531137350353504, -34.99999999999999289, 101.0054374292562187 ) ) ;
#2548 = DIRECTION ( 'NONE',  ( -0.000000000000000000, -1.000000000000000000, -0.000000000000000000 ) ) ;
#2549 = DIRECTION ( 'NONE',  ( 0.000000000000000000, 0.000000000000000000, 1.000000000000000000 ) ) ;
#2550 = VERTEX_POINT ( 'NONE', #10284 ) ;
#2551 = CARTESIAN_POINT ( 'NONE',  ( 229.5999999999999375, -34.53749999999999432, -51.73205080756898866 ) ) ;
#2552 = CARTESIAN_POINT ( 'NONE',  ( -82.39999999999999147, -30.70312499938548711, -103.1828516163667899 ) ) ;
#2553 = VECTOR ( 'NONE', #2515, 1000.000000000000000 ) ;
#2554 = AXIS2_PLACEMENT_3D ( 'NONE', #5082, #11024, #13955 ) ;
#2555 = CARTESIAN_POINT ( 'NONE',  ( 3.973110223767137850, -2.261515145575163828E-11, -3.565797985667433778 ) ) ;
#2556 = CARTESIAN_POINT ( 'NONE',  ( -83.20384757729335945, -34.85759618943233562, -96.99999999999998579 ) ) ;
#2557 = CARTESIAN_POINT ( 'NONE',  ( -83.77821517812500929, -32.87812499938548427, 102.3871387122750889 ) ) ;
#2558 = DIRECTION ( 'NONE',  ( -7.222237291452147586E-32, 1.214306433183764966E-16, -1.000000000000000000 ) ) ;
#2559 = CARTESIAN_POINT ( 'NONE',  ( 232.5999999999999375, -30.25312499938548072, -53.18285161636690361 ) ) ;
#2560 = EDGE_CURVE ( 'NONE', #17012, #5681, #1910, .T. ) ;
#2561 = EDGE_LOOP ( 'NONE', ( #3567, #17100, #10119, #4108 ) ) ;
#2562 = CARTESIAN_POINT ( 'NONE',  ( -81.02178482187500208, -33.89062499938548711, 97.61286128772489690 ) ) ;
#2563 = EDGE_CURVE ( 'NONE', #11976, #6642, #13389, .T. ) ;
#2564 = CARTESIAN_POINT ( 'NONE',  ( -80.90000000000000568, -30.69374999877097210, 102.5980762113533018 ) ) ;
#2565 = CARTESIAN_POINT ( 'NONE',  ( 79.64356964375001269, -34.37812499938548427, 101.5914258081833879 ) ) ;
#2566 = CARTESIAN_POINT ( 'NONE',  ( 94.79999999999984084, 0.000000000000000000, 150.0000000000000000 ) ) ;
#2568 = CARTESIAN_POINT ( 'NONE',  ( 233.9782151781249411, -32.54062499938547859, 97.61286128772489690 ) ) ;
#2567 = VECTOR ( 'NONE', #9890, 1000.000000000000000 ) ;
#2569 = DIRECTION ( 'NONE',  ( 1.000000000000000000, -1.387778780781445676E-15, -2.407412430484046130E-31 ) ) ;
#2570 =( BOUNDED_CURVE ( )  B_SPLINE_CURVE ( 2, ( #16733, #2176, #5116, #16641, #18495, #12335, #11056, #1881, #8133, #3541, #10768, #10961, #344, #9598, #16838, #15562, #17026, #3341, #18399, #15464, #1979, #14085, #10671, #1783, #4920, #15361, #9202, #7936, #5020, #13989, #6383, #6197, #9302, #2075, #4728, #12146, #15266, #10866, #526, #6291, #8031, #9398, #13887, #4827, #15166, #7747, #18114, #7840, #3444, #18209, #12524, #13794, #18302, #16930, #439, #6479, #12432, #13704, #9497, #12240, #628, #6576, #3637, #11352, #1091, #15754, #4029, #817, #16039, #5210, #15658, #18784, #9891, #3731, #2462, #12914, #8508, #914, #2640, #11254, #9989, #8233, #5313 ),
 .UNSPECIFIED., .F., .F. ) 
 B_SPLINE_CURVE_WITH_KNOTS ( ( 3, 2, 2, 2, 2, 2, 2, 2, 2, 2, 2, 2, 2, 2, 2, 2, 2, 2, 2, 2, 2, 2, 2, 2, 2, 2, 2, 2, 2, 2, 2, 2, 2, 2, 2, 2, 2, 2, 2, 2, 2, 3 ),
 ( 0.3495698921800940995, 0.3600184345287980037, 0.3750192026341646057, 0.3900199707395312076, 0.4050207388448978096, 0.4200215069502644116, 0.4350222750556309581, 0.4500230431609975601, 0.4650238112663641621, 0.4800245793717307086, 0.4950253474770972550, 0.5100261155824639125, 0.5250268836878304590, 0.5400276517931970055, 0.5550284198985635520, 0.5700291880039302095, 0.5850299561092967560, 0.6000307242146634135, 0.6150314923200299599, 0.6300322604253966174, 0.6450330285307630529, 0.6600337966361298214, 0.6750345647414963679, 0.6900353328468629144, 0.7050361009522294609, 0.7200368690575960073, 0.7350376371629626648, 0.7500384052683292113, 0.7650391733736958688, 0.7800399414790624153, 0.7950407095844290728, 0.8100414776897955083, 0.8250422457951620547, 0.8400430139005288233, 0.8550437820058953697, 0.8700445501112619162, 0.8850453182166284627, 0.9000460863219950092, 0.9150468544273615557, 0.9300476225327283242, 0.9450483906380948707, 0.9496006163947574574 ),
 .UNSPECIFIED. ) 
 CURVE ( )  GEOMETRIC_REPRESENTATION_ITEM ( )  RATIONAL_B_SPLINE_CURVE ( ( 0.9433623850486894113, 0.9066821623815382036, 1.000000000000000000, 0.8660254037844387076, 1.000000000000000000, 0.8660254037844387076, 1.000000000000000000, 0.8660254037844387076, 1.000000000000000000, 0.8660254037844387076, 1.000000000000000000, 0.8660254037844387076, 1.000000000000000000, 0.8660254037844387076, 1.000000000000000000, 0.8660254037844387076, 1.000000000000000000, 0.8660254037844387076, 1.000000000000000000, 0.8660254037844387076, 1.000000000000000000, 0.8660254037844387076, 1.000000000000000000, 0.8660254037844387076, 1.000000000000000000, 0.8660254037844387076, 1.000000000000000000, 0.8660254037844387076, 1.000000000000000000, 0.8660254037844387076, 1.000000000000000000, 0.8660254037844387076, 1.000000000000000000, 0.8660254037844387076, 1.000000000000000000, 0.8660254037844387076, 1.000000000000000000, 0.8660254037844387076, 1.000000000000000000, 0.8660254037844387076, 1.000000000000000000, 0.8660254037844387076, 1.000000000000000000, 0.8660254037844387076, 1.000000000000000000, 0.8660254037844387076, 1.000000000000000000, 0.8660254037844387076, 1.000000000000000000, 0.8660254037844387076, 1.000000000000000000, 0.8660254037844387076, 1.000000000000000000, 0.8660254037844387076, 1.000000000000000000, 0.8660254037844387076, 1.000000000000000000, 0.8660254037844387076, 1.000000000000000000, 0.8660254037844387076, 1.000000000000000000, 0.8660254037844387076, 1.000000000000000000, 0.8660254037844387076, 1.000000000000000000, 0.8660254037844387076, 1.000000000000000000, 0.8660254037844387076, 1.000000000000000000, 0.8660254037844387076, 1.000000000000000000, 0.8660254037844387076, 1.000000000000000000, 0.8660254037844387076, 1.000000000000000000, 0.8660254037844387076, 1.000000000000000000, 0.8660254037844387076, 1.000000000000000000, 0.8660254037844387076, 1.000000000000000000, 0.9593432414029002819, 0.9433623850486891893 ) ) 
 REPRESENTATION_ITEM ( '' )  );
#2571 = CARTESIAN_POINT ( 'NONE',  ( -79.64356964374998427, -33.59062499938548285, 98.40857419181659793 ) ) ;
#2572 = CARTESIAN_POINT ( 'NONE',  ( -79.64356964374998427, -33.59062499938548285, -101.5914258081833879 ) ) ;
#2573 = CARTESIAN_POINT ( 'NONE',  ( 82.39999999999999147, -34.75312499938549138, 103.1828516163667899 ) ) ;
#2574 = CARTESIAN_POINT ( 'NONE',  ( 85.15643035624999868, -33.44062499938548427, -98.40857419181659793 ) ) ;
#2575 = ADVANCED_FACE ( 'NONE', ( #8900 ), #4713, .F. ) ;
#2576 = CARTESIAN_POINT ( 'NONE',  ( 229.8435696437499871, -34.15312499938547575, -48.40857419181671162 ) ) ;
#2577 = CARTESIAN_POINT ( 'NONE',  ( -79.64356964374998427, -32.57812499938548711, 98.40857419181659793 ) ) ;
#2578 = CARTESIAN_POINT ( 'NONE',  ( 85.15643035624999868, -31.52812499938547930, -98.40857419181659793 ) ) ;
#2579 = VERTEX_POINT ( 'NONE', #6181 ) ;
#2580 = CYLINDRICAL_SURFACE ( 'NONE', #8809, 3.000000000000002665 ) ;
#2581 = DIRECTION ( 'NONE',  ( -0.000000000000000000, -1.000000000000000000, -0.000000000000000000 ) ) ;
#2582 = CARTESIAN_POINT ( 'NONE',  ( -82.39999999999999147, -32.81250000000000000, 96.53589838486223584 ) ) ;
#2583 = CARTESIAN_POINT ( 'NONE',  ( -85.15643035625001289, -34.19062499938548427, 99.99999999999998579 ) ) ;
#2584 = CARTESIAN_POINT ( 'NONE',  ( -79.64356964375001269, -31.22812499938548925, 98.40857419181659793 ) ) ;
#2585 = EDGE_LOOP ( 'NONE', ( #7926, #17793, #18316 ) ) ;
#2586 = DIRECTION ( 'NONE',  ( -0.000000000000000000, -1.000000000000000000, -0.000000000000000000 ) ) ;
#2587 = CARTESIAN_POINT ( 'NONE',  ( 235.3564303562499447, -33.06562499938547717, 99.99999999999998579 ) ) ;
#2588 = CARTESIAN_POINT ( 'NONE',  ( 79.77811200999867935, -34.99999999999999289, -100.8506536761476013 ) ) ;
#2589 = CARTESIAN_POINT ( 'NONE',  ( 85.40000000000000568, -33.63750000000000284, -98.26794919243111792 ) ) ;
#2590 = ADVANCED_FACE ( 'NONE', ( #12132 ), #14862, .T. ) ;
#2591 = DIRECTION ( 'NONE',  ( 1.000000000000000000, 0.000000000000000000, 0.000000000000000000 ) ) ;
#2592 = CARTESIAN_POINT ( 'NONE',  ( 1.567478505476134606E-15, 4.618802153517012066, -3.433295621305382905 ) ) ;
#2593 = CARTESIAN_POINT ( 'NONE',  ( -83.77821517812500929, -30.21562499938548285, 97.61286128772489690 ) ) ;
#2594 = DIRECTION ( 'NONE',  ( 2.312964634635736745E-15, 1.000000000000000000, 0.000000000000000000 ) ) ;
#2595 = CARTESIAN_POINT ( 'NONE',  ( 79.64356964375001269, -30.51562499938548711, 98.40857419181659793 ) ) ;
#2596 = CARTESIAN_POINT ( 'NONE',  ( 233.7735609739808353, -32.00000000000002132, 97.33634050170194030 ) ) ;
#2597 = CARTESIAN_POINT ( 'NONE',  ( 105.2000000000001307, -29.80000000000002203, 147.7999999999999829 ) ) ;
#2598 = CARTESIAN_POINT ( 'NONE',  ( 85.15643035624999868, -34.34062499938548285, -98.40857419181659793 ) ) ;
#2599 = PLANE ( 'NONE',  #2724 ) ;
#2600 = ORIENTED_EDGE ( 'NONE', *, *, #13152, .F. ) ;
#2601 = CARTESIAN_POINT ( 'NONE',  ( 85.40000000000000568, -32.19374999877096855, 99.99999999999998579 ) ) ;
#2602 = CONTEXT_DEPENDENT_SHAPE_REPRESENTATION ( #4847, #12628 ) ;
#2603 = CARTESIAN_POINT ( 'NONE',  ( 233.9782151781249411, -34.45312499938548001, 97.61286128772489690 ) ) ;
#2604 = CARTESIAN_POINT ( 'NONE',  ( 231.2217848218749339, -33.92812499938548143, -52.38713871227520968 ) ) ;
#2605 =( BOUNDED_CURVE ( )  B_SPLINE_CURVE ( 1, ( #1455, #6243 ),
 .UNSPECIFIED., .F., .F. ) 
 B_SPLINE_CURVE_WITH_KNOTS ( ( 2, 2 ),
 ( 0.000000000000000000, 1.000000000000000000 ),
 .UNSPECIFIED. ) 
 CURVE ( )  GEOMETRIC_REPRESENTATION_ITEM ( )  RATIONAL_B_SPLINE_CURVE ( ( 0.9401542295229963209, 0.9401542295229963209 ) ) 
 REPRESENTATION_ITEM ( '' )  );
#2606 = CARTESIAN_POINT ( 'NONE',  ( 83.90000000000000568, -34.42500000000000426, 97.40192378864668399 ) ) ;
#2607 = FACE_OUTER_BOUND ( 'NONE', #15254, .T. ) ;
#2608 = EDGE_LOOP ( 'NONE', ( #14282, #8327, #16343, #15423 ) ) ;
#2609 = CARTESIAN_POINT ( 'NONE',  ( -79.64356964375001269, -33.02812499938548285, -101.5914258081833879 ) ) ;
#2610 = CYLINDRICAL_SURFACE ( 'NONE', #6627, 3.000000000000002665 ) ;
#2611 = ORIENTED_EDGE ( 'NONE', *, *, #17471, .T. ) ;
#2612 = CARTESIAN_POINT ( 'NONE',  ( 79.64356964374999848, -34.97812499938548569, 99.99999999999998579 ) ) ;
#2613 = CARTESIAN_POINT ( 'NONE',  ( -83.77821517812500929, -31.52812499938548996, -97.61286128772489690 ) ) ;
#2614 = CARTESIAN_POINT ( 'NONE',  ( 83.33080762004576059, -35.05289549976084373, 103.5578907812544855 ) ) ;
#2615 = CARTESIAN_POINT ( 'NONE',  ( -79.73531137350346398, -34.99999999999999289, 98.99456257074389498 ) ) ;
#2616 = CARTESIAN_POINT ( 'NONE',  ( -82.39999999999999147, -30.51018749875868252, 96.53589838486223584 ) ) ;
#2617 = CARTESIAN_POINT ( 'NONE',  ( -79.64356964375001269, -31.79062499938548569, 98.40857419181659793 ) ) ;
#2618 = LINE ( 'NONE', #8579, #19133 ) ;
#2619 = CARTESIAN_POINT ( 'NONE',  ( 5.599999999999999645, 2.020725942163686728, -3.499999999999999556 ) ) ;
#2620 = CARTESIAN_POINT ( 'NONE',  ( 82.39999999999999147, -31.63124999877097210, -103.4641016151377499 ) ) ;
#2621 = CARTESIAN_POINT ( 'NONE',  ( 234.0999999999999375, -30.74999999999999645, 102.5980762113533018 ) ) ;
#2622 = VERTEX_POINT ( 'NONE', #13203 ) ;
#2623 = CARTESIAN_POINT ( 'NONE',  ( 231.2217848218749339, -32.12812499938547717, -52.38713871227520968 ) ) ;
#2624 =( NAMED_UNIT ( * ) PLANE_ANGLE_UNIT ( ) SI_UNIT ( $, .RADIAN. ) );
#2625 = CARTESIAN_POINT ( 'NONE',  ( 235.5999999999999375, -32.41874999877096286, 99.99999999999998579 ) ) ;
#2626 = CARTESIAN_POINT ( 'NONE',  ( 235.5999999999999943, -31.48124999877096286, -51.73205080756900287 ) ) ;
#2627 = CARTESIAN_POINT ( 'NONE',  ( -82.39999999999999147, -31.82812499938548356, 103.1828516163667899 ) ) ;
#2628 = ORIENTED_EDGE ( 'NONE', *, *, #2320, .F. ) ;
#2629 = EDGE_LOOP ( 'NONE', ( #3384, #9873, #14255, #8421 ) ) ;
#2630 = CARTESIAN_POINT ( 'NONE',  ( -81.59615242270663771, -32.11740381056766580, 103.0000000000000000 ) ) ;
#2631 = VECTOR ( 'NONE', #15371, 1000.000000000000000 ) ;
#2632 = DIRECTION ( 'NONE',  ( 1.000000000000000000, 0.000000000000000000, 0.000000000000000000 ) ) ;
#2633 = ORIENTED_EDGE ( 'NONE', *, *, #645, .T. ) ;
#2634 = FACE_OUTER_BOUND ( 'NONE', #12321, .T. ) ;
#2635 = CARTESIAN_POINT ( 'NONE',  ( 85.40000000000000568, -32.73750000000000426, -98.26794919243111792 ) ) ;
#2636 = CARTESIAN_POINT ( 'NONE',  ( -82.39999999999999147, -33.48750000000000426, 103.0000000000000000 ) ) ;
#2637 = CARTESIAN_POINT ( 'NONE',  ( -82.39999999999999147, -32.16562499938549280, 96.81714838363319586 ) ) ;
#2638 = CARTESIAN_POINT ( 'NONE',  ( -79.39999999999999147, -31.08750000000000213, 98.26794919243110371 ) ) ;
#2639 = CARTESIAN_POINT ( 'NONE',  ( -79.39999999999999147, -34.68750000000000000, -101.7320508075688963 ) ) ;
#2640 = CARTESIAN_POINT ( 'NONE',  ( 81.02178482187500208, -34.90312499938548285, -97.61286128772489690 ) ) ;
#2641 = CARTESIAN_POINT ( 'NONE',  ( 80.48808202378427268, -35.00000000000000000, 102.1951992292041638 ) ) ;
#2642 = CARTESIAN_POINT ( 'NONE',  ( -81.02178482187500208, -34.49062499938548854, 102.3871387122750889 ) ) ;
#2643 = CARTESIAN_POINT ( 'NONE',  ( 111.0000000000000000, 10.19999999999997620, -139.9999999999999716 ) ) ;
#2644 = VERTEX_POINT ( 'NONE', #19175 ) ;
#2645 =( NAMED_UNIT ( * ) SI_UNIT ( $, .STERADIAN. ) SOLID_ANGLE_UNIT ( ) );
#2646 = CARTESIAN_POINT ( 'NONE',  ( -82.39999999999999147, -30.92812499938548143, -96.81714838363319586 ) ) ;
#2647 = CARTESIAN_POINT ( 'NONE',  ( 235.3058334582607074, -35.00000000000002132, 100.6274906301342327 ) ) ;
#2648 = EDGE_CURVE ( 'NONE', #13696, #4492, #3094, .T. ) ;
#2649 = AXIS2_PLACEMENT_3D ( 'NONE', #7712, #1755, #9366 ) ;
#2650 = CARTESIAN_POINT ( 'NONE',  ( -1.243802165048909503, 3.900692638707381921, -3.223146290109805800 ) ) ;
#2651 =( BOUNDED_CURVE ( )  B_SPLINE_CURVE ( 2, ( #8921, #10589, #13604, #5811, #16554, #5911, #1513 ),
 .UNSPECIFIED., .F., .F. ) 
 B_SPLINE_CURVE_WITH_KNOTS ( ( 3, 2, 2, 3 ),
 ( 0.8958333333333333703, 0.9027777777777777901, 0.9166666666666666297, 0.9258785066912882389 ),
 .UNSPECIFIED. ) 
 CURVE ( )  GEOMETRIC_REPRESENTATION_ITEM ( )  RATIONAL_B_SPLINE_CURVE ( ( 0.9330127018922192983, 0.9330127018922198534, 1.000000000000000000, 0.8660254037844387076, 1.000000000000000000, 0.9111410165655264848, 0.9401539157124900736 ) ) 
 REPRESENTATION_ITEM ( '' )  );
#2652 = DIRECTION ( 'NONE',  ( 1.000000000000000000, 0.000000000000000000, 0.000000000000000000 ) ) ;
#2653 = CARTESIAN_POINT ( 'NONE',  ( -79.64356964374999848, -30.81562499938548427, 99.99999999999998579 ) ) ;
#2654 = CARTESIAN_POINT ( 'NONE',  ( 81.59615242270662350, -32.56740381056766864, 97.00000000000000000 ) ) ;
#2655 = CARTESIAN_POINT ( 'NONE',  ( 229.8435696437499303, -32.84062499938547575, -50.00000000000011369 ) ) ;
#2656 = EDGE_CURVE ( 'NONE', #15452, #3491, #13298, .T. ) ;
#2657 = EDGE_CURVE ( 'NONE', #5317, #2292, #11838, .T. ) ;
#2658 = VERTEX_POINT ( 'NONE', #17904 ) ;
#2659 = CARTESIAN_POINT ( 'NONE',  ( -82.39999999999999147, -33.40312499938548285, 96.81714838363319586 ) ) ;
#2660 = CARTESIAN_POINT ( 'NONE',  ( -79.39999999999999147, -33.86250000000000426, -98.26794919243113213 ) ) ;
#2661 = CARTESIAN_POINT ( 'NONE',  ( 85.15643035625001289, -34.64062499938548711, 99.99999999999998579 ) ) ;
#2662 = CARTESIAN_POINT ( 'NONE',  ( 0.1217565302851102982, 3.710888496608919507, -0.5725525826504667126 ) ) ;
#2663 = CARTESIAN_POINT ( 'NONE',  ( 235.3564303562499447, -30.32812499938548001, 98.40857419181659793 ) ) ;
#2664 = CARTESIAN_POINT ( 'NONE',  ( 233.9782151781249411, -32.24062499938548143, -47.61286128772501769 ) ) ;
#2665 = CARTESIAN_POINT ( 'NONE',  ( -99.99999999999998579, -5.200000000000000178, -150.0000000000000000 ) ) ;
#2666 = CARTESIAN_POINT ( 'NONE',  ( -79.64356964374999848, -33.17812499938548854, -99.99999999999998579 ) ) ;
#2667 = CARTESIAN_POINT ( 'NONE',  ( 79.64356964375001269, -33.92812499938548854, 101.5914258081833879 ) ) ;
#2668 = EDGE_CURVE ( 'NONE', #6163, #15956, #5228, .T. ) ;
#2669 = CARTESIAN_POINT ( 'NONE',  ( 83.77821517812500929, -34.67812499938548854, -102.3871387122750889 ) ) ;
#2670 = CARTESIAN_POINT ( 'NONE',  ( 232.5999999999999375, -30.78749999999999432, -46.53589838486234953 ) ) ;
#2671 = EDGE_CURVE ( 'NONE', #19154, #12568, #4037, .T. ) ;
#2672 = CARTESIAN_POINT ( 'NONE',  ( -85.15643035625001289, -32.84062499938548285, 99.99999999999998579 ) ) ;
#2673 = CARTESIAN_POINT ( 'NONE',  ( 79.64356964375001269, -31.22812499938548925, -98.40857419181659793 ) ) ;
#2674 = ADVANCED_FACE ( 'NONE', ( #2162 ), #424, .T. ) ;
#2675 = ORIENTED_EDGE ( 'NONE', *, *, #1608, .F. ) ;
#2676 = CARTESIAN_POINT ( 'NONE',  ( 85.15643035624999868, -34.79062499938548569, 101.5914258081833879 ) ) ;
#2677 = DIRECTION ( 'NONE',  ( 0.000000000000000000, 0.000000000000000000, 1.000000000000000000 ) ) ;
#2678 = B_SPLINE_CURVE_WITH_KNOTS ( 'NONE', 3,
 ( #2834, #1183, #11537, #15, #17499, #11626 ),
 .UNSPECIFIED., .F., .F.,
 ( 4, 2, 4 ),
 ( 0.002452478801916376308, 0.003676905084148007850, 0.004901331366379639391 ),
 .UNSPECIFIED. ) ;
#2679 = CARTESIAN_POINT ( 'NONE',  ( -83.90000000000000568, -32.62500000000000000, 102.5980762113533018 ) ) ;
#2680 = AXIS2_PLACEMENT_3D ( 'NONE', #9321, #2287, #15484 ) ;
#2681 = CARTESIAN_POINT ( 'NONE',  ( -79.64356964374999848, -33.51562499938548711, 99.99999999999998579 ) ) ;
#2682 = ORIENTED_EDGE ( 'NONE', *, *, #4144, .F. ) ;
#2683 = CARTESIAN_POINT ( 'NONE',  ( -83.20384757729335945, -33.90134618820329848, 102.9999999999999716 ) ) ;
#2685 = LINE ( 'NONE', #9930, #9733 ) ;
#2684 =( BOUNDED_CURVE ( )  B_SPLINE_CURVE ( 2, ( #3057, #13509, #146, #17819, #4429, #9108, #12044, #1692, #11660 ),
 .UNSPECIFIED., .F., .F. ) 
 B_SPLINE_CURVE_WITH_KNOTS ( ( 3, 2, 2, 2, 3 ),
 ( 0.3125000000000001665, 0.3194444444444444198, 0.3333333333333333148, 0.3472222222222222099, 0.3541666666666666297 ),
 .UNSPECIFIED. ) 
 CURVE ( )  GEOMETRIC_REPRESENTATION_ITEM ( )  RATIONAL_B_SPLINE_CURVE ( ( 0.9330127018922194093, 0.9330127018922209636, 1.000000000000000000, 0.8660254037844387076, 1.000000000000000000, 0.8660254037844387076, 1.000000000000000000, 0.9330127018922196314, 0.9330127018922194093 ) ) 
 REPRESENTATION_ITEM ( '' )  );
#2686 = CARTESIAN_POINT ( 'NONE',  ( 79.91954014136219087, -34.99999999999998579, -98.55723758691000569 ) ) ;
#2687 = CARTESIAN_POINT ( 'NONE',  ( -82.39999999999999147, -30.10856250001229384, 96.53589838486223584 ) ) ;
#2688 = AXIS2_PLACEMENT_3D ( 'NONE', #300, #18165, #13754 ) ;
#2689 = CARTESIAN_POINT ( 'NONE',  ( -82.39999999999999147, -34.83749999999999858, 103.0000000000000000 ) ) ;
#2690 = CARTESIAN_POINT ( 'NONE',  ( -81.59615242270662350, -32.96115380933864003, 103.0000000000000000 ) ) ;
#2691 = LINE ( 'NONE', #11299, #11643 ) ;
#2692 = CARTESIAN_POINT ( 'NONE',  ( -83.90000000000000568, -32.56874999877096855, 102.5980762113533018 ) ) ;
#2693 = CARTESIAN_POINT ( 'NONE',  ( 79.64356964374999848, -32.72812499938548569, 99.99999999999998579 ) ) ;
#2694 = CARTESIAN_POINT ( 'NONE',  ( 230.7186334667983658, -32.00000000000000711, 97.98546077809203325 ) ) ;
#2695 = CARTESIAN_POINT ( 'NONE',  ( 231.7961524227065411, -33.05759618943232425, -47.00000000000012790 ) ) ;
#2696 = CARTESIAN_POINT ( 'NONE',  ( 83.77821517812500929, -34.67812499938548854, -102.3871387122750889 ) ) ;
#2697 = CARTESIAN_POINT ( 'NONE',  ( 229.5999999999999375, -34.04999999999999716, 99.99999999999998579 ) ) ;
#2698 = ORIENTED_EDGE ( 'NONE', *, *, #15683, .F. ) ;
#2699 = ADVANCED_FACE ( 'NONE', ( #16824, #10946, #12223 ), #11043, .T. ) ;
#2700 = CARTESIAN_POINT ( 'NONE',  ( 85.40000000000000568, -32.23124999877096997, 101.7320508075688679 ) ) ;
#2701 = CARTESIAN_POINT ( 'NONE',  ( 233.9782151781249411, -34.90312499938547575, 97.61286128772489690 ) ) ;
#2702 = EDGE_CURVE ( 'NONE', #4468, #10833, #1964, .T. ) ;
#2703 = CARTESIAN_POINT ( 'NONE',  ( 235.3564303562499447, -34.52812499938547575, -50.00000000000011369 ) ) ;
#2704 = CARTESIAN_POINT ( 'NONE',  ( -83.77821517812500929, -33.32812499938548711, -97.61286128772489690 ) ) ;
#2705 = LINE ( 'NONE', #19224, #5247 ) ;
#2706 = LINE ( 'NONE', #180, #17740 ) ;
#2707 = ORIENTED_EDGE ( 'NONE', *, *, #8266, .T. ) ;
#2708 = CARTESIAN_POINT ( 'NONE',  ( -81.02178482187500208, -33.89062499938548711, -102.3871387122750889 ) ) ;
#2709 = AXIS2_PLACEMENT_3D ( 'NONE', #15635, #9768, #11129 ) ;
#2710 = DIRECTION ( 'NONE',  ( -0.000000000000000000, -0.000000000000000000, -1.000000000000000000 ) ) ;
#2711 = ORIENTED_EDGE ( 'NONE', *, *, #8413, .T. ) ;
#2712 = CARTESIAN_POINT ( 'NONE',  ( 83.77821517812500929, -34.82812499938548711, 102.3871387122750889 ) ) ;
#2713 = ADVANCED_FACE ( 'NONE', ( #15547 ), #15346, .T. ) ;
#2714 = CARTESIAN_POINT ( 'NONE',  ( -85.15643035624999868, -31.19062499938548783, -101.5914258081833879 ) ) ;
#2715 = CARTESIAN_POINT ( 'NONE',  ( -82.39999999999999147, -31.85624999877097352, -103.4641016151377499 ) ) ;
#2716 = CARTESIAN_POINT ( 'NONE',  ( 231.2217848218749339, -32.12812499938547717, 97.61286128772489690 ) ) ;
#2717 = CARTESIAN_POINT ( 'NONE',  ( -83.90000000000000568, -30.47268749875867755, 97.40192378864668399 ) ) ;
#2718 = TOROIDAL_SURFACE ( 'NONE', #18020, 5.200000000000001066, 0.4999999999999978351 ) ;
#2719 = CARTESIAN_POINT ( 'NONE',  ( -81.02178482187500208, -31.30312499938548498, 97.61286128772489690 ) ) ;
#2720 = CARTESIAN_POINT ( 'NONE',  ( -85.15643035625001289, -32.39062499938548711, -99.99999999999998579 ) ) ;
#2721 = FACE_OUTER_BOUND ( 'NONE', #1011, .T. ) ;
#2722 = DIRECTION ( 'NONE',  ( -0.000000000000000000, -0.000000000000000000, -1.000000000000000000 ) ) ;
#2723 = CARTESIAN_POINT ( 'NONE',  ( 85.40000000000000568, -32.19374999877096855, -99.99999999999998579 ) ) ;
#2724 = AXIS2_PLACEMENT_3D ( 'NONE', #15994, #17559, #6920 ) ;
#2725 = CARTESIAN_POINT ( 'NONE',  ( 234.0999999999999375, -30.14999999999999503, 97.40192378864668399 ) ) ;
#2726 =( BOUNDED_CURVE ( )  B_SPLINE_CURVE ( 2, ( #11190, #17153, #3761, #15690, #4440, #16459, #5816, #2782, #8833 ),
 .UNSPECIFIED., .F., .F. ) 
 B_SPLINE_CURVE_WITH_KNOTS ( ( 3, 2, 2, 2, 3 ),
 ( 0.4375000000000001110, 0.4444444444444444198, 0.4583333333333333148, 0.4722222222222222099, 0.4791666666666666852 ),
 .UNSPECIFIED. ) 
 CURVE ( )  GEOMETRIC_REPRESENTATION_ITEM ( )  RATIONAL_B_SPLINE_CURVE ( ( 0.9330127018922194093, 0.9330127018922204085, 1.000000000000000000, 0.8660254037844387076, 1.000000000000000000, 0.8660254037844387076, 1.000000000000000000, 0.9330127018922190762, 0.9330127018922194093 ) ) 
 REPRESENTATION_ITEM ( '' )  );
#2727 = ORIENTED_EDGE ( 'NONE', *, *, #13319, .T. ) ;
#2728 = CARTESIAN_POINT ( 'NONE',  ( 83.20395887649171129, -35.00000000000000711, -102.6365808225363878 ) ) ;
#2729 = CARTESIAN_POINT ( 'NONE',  ( 232.5999999999999375, -33.20624999877095718, 96.53589838486223584 ) ) ;
#2730 = CARTESIAN_POINT ( 'NONE',  ( 234.0999999999999375, -33.69374999877096144, -52.59807621135342970 ) ) ;
#2731 = CARTESIAN_POINT ( 'NONE',  ( -81.02178482187500208, -30.29062499938548569, 97.61286128772489690 ) ) ;
#2732 = VECTOR ( 'NONE', #4812, 1000.000000000000000 ) ;
#2733 = ORIENTED_EDGE ( 'NONE', *, *, #2503, .T. ) ;
#2734 = ORIENTED_EDGE ( 'NONE', *, *, #9238, .F. ) ;
#2735 = DIRECTION ( 'NONE',  ( 0.000000000000000000, 0.000000000000000000, 1.000000000000000000 ) ) ;
#2736 = DIRECTION ( 'NONE',  ( -1.586032892321652088E-15, -1.000000000000000000, 0.000000000000000000 ) ) ;
#2737 = DIRECTION ( 'NONE',  ( -1.000000000000000000, 6.244088828561840598E-46, 1.735459783503185124E-31 ) ) ;
#2738 = VERTEX_POINT ( 'NONE', #18288 ) ;
#2739 = CARTESIAN_POINT ( 'NONE',  ( -82.39999999999999147, -31.85624999877096641, 96.99999999999998579 ) ) ;
#2740 = CARTESIAN_POINT ( 'NONE',  ( 79.39999999999999147, -34.68750000000000000, -98.26794919243110371 ) ) ;
#2741 = CARTESIAN_POINT ( 'NONE',  ( 2.500000000000000444, 0.000000000000000000, -5.000000000000000888 ) ) ;
#2742 = VECTOR ( 'NONE', #8367, 1000.000000000000000 ) ;
#2743 = CARTESIAN_POINT ( 'NONE',  ( -85.15643035624999868, -30.74062499938548143, 98.40857419181659793 ) ) ;
#2744 = CARTESIAN_POINT ( 'NONE',  ( -79.39999999999999147, -32.92500000000000426, 99.99999999999998579 ) ) ;
#2745 = CARTESIAN_POINT ( 'NONE',  ( 233.4038475772933054, -32.51115380933862298, -47.00000000000010658 ) ) ;
#2746 = PRESENTATION_STYLE_ASSIGNMENT (( #10173 ) ) ;
#2747 = AXIS2_PLACEMENT_3D ( 'NONE', #17009, #11044, #3328 ) ;
#2748 = DIRECTION ( 'NONE',  ( 0.000000000000000000, 0.000000000000000000, -1.000000000000000000 ) ) ;
#2749 = LINE ( 'NONE', #8607, #13353 ) ;
#2750 = CYLINDRICAL_SURFACE ( 'NONE', #7410, 2.649999999999985700 ) ;
#2751 = ORIENTED_EDGE ( 'NONE', *, *, #7602, .T. ) ;
#2752 = PRESENTATION_STYLE_ASSIGNMENT (( #11646 ) ) ;
#2753 = CARTESIAN_POINT ( 'NONE',  ( -85.15643035625001289, -35.20312499938548711, -99.99999999999998579 ) ) ;
#2754 = CARTESIAN_POINT ( 'NONE',  ( 232.5999999999999375, -33.20624999877097139, -53.00000000000011369 ) ) ;
#2755 = VECTOR ( 'NONE', #4872, 1000.000000000000000 ) ;
#2756 = AXIS2_PLACEMENT_3D ( 'NONE', #6720, #16883, #1834 ) ;
#2757 = CARTESIAN_POINT ( 'NONE',  ( -79.39999999999999147, -33.28124999877096712, 98.26794919243110371 ) ) ;
#2758 = CARTESIAN_POINT ( 'NONE',  ( 235.2218879900010791, -35.00000000000000000, 100.8506536761482124 ) ) ;
#2759 = CARTESIAN_POINT ( 'NONE',  ( -83.77821517812500929, -31.56562499938548427, 97.61286128772489690 ) ) ;
#2760 = DIRECTION ( 'NONE',  ( 0.8660254037844378194, -0.5000000000000015543, -6.071532165918849482E-17 ) ) ;
#2761 = CARTESIAN_POINT ( 'NONE',  ( 233.9782151781249411, -32.09062499938547575, -52.38713871227520968 ) ) ;
#2762 = VERTEX_POINT ( 'NONE', #511 ) ;
#2763 = ORIENTED_EDGE ( 'NONE', *, *, #1169, .F. ) ;
#2764 = CARTESIAN_POINT ( 'NONE',  ( -84.56803305035340657, -32.00000000000000000, 101.7116913729794305 ) ) ;
#2765 = CARTESIAN_POINT ( 'NONE',  ( -85.15643035624999868, -33.25312499938548427, 101.5914258081833879 ) ) ;
#2766 = CARTESIAN_POINT ( 'NONE',  ( 232.5999999999999375, -33.43124999877096570, -47.00000000000011369 ) ) ;
#2767 = CARTESIAN_POINT ( 'NONE',  ( 83.88339518848731302, -35.16733441503058089, 102.5204086375588162 ) ) ;
#2768 = CARTESIAN_POINT ( 'NONE',  ( 85.40000000000000568, -34.01250000000000284, -101.7320508075688821 ) ) ;
#2769 = AXIS2_PLACEMENT_3D ( 'NONE', #14325, #2504, #1145 ) ;
#2770 = CARTESIAN_POINT ( 'NONE',  ( 231.2217848218749339, -30.51562499938548001, 102.3871387122750889 ) ) ;
#2771 = CARTESIAN_POINT ( 'NONE',  ( 235.3564303562499447, -34.90312499938547575, -48.40857419181671162 ) ) ;
#2772 = PLANE ( 'NONE',  #11462 ) ;
#2773 = CARTESIAN_POINT ( 'NONE',  ( 83.77821517812500929, -35.01562499938548711, 97.61286128772489690 ) ) ;
#2774 = EDGE_CURVE ( 'NONE', #15407, #14034, #5192, .T. ) ;
#2775 = EDGE_CURVE ( 'NONE', #18799, #19181, #50, .T. ) ;
#2776 = CARTESIAN_POINT ( 'NONE',  ( 81.02178482187500208, -31.34062499938548996, -102.3871387122750889 ) ) ;
#2777 = CARTESIAN_POINT ( 'NONE',  ( 229.5999999999999375, -30.03749999999999432, -51.73205080756898866 ) ) ;
#2778 = CARTESIAN_POINT ( 'NONE',  ( -79.64356964374998427, -33.47812499938547859, 98.40857419181659793 ) ) ;
#2779 = CARTESIAN_POINT ( 'NONE',  ( 85.15643035624999868, -31.97812499938548925, -98.40857419181659793 ) ) ;
#2780 = ORIENTED_EDGE ( 'NONE', *, *, #6300, .T. ) ;
#2781 = DIRECTION ( 'NONE',  ( -0.000000000000000000, -1.000000000000000000, -0.000000000000000000 ) ) ;
#2782 = CARTESIAN_POINT ( 'NONE',  ( 233.4038475772933054, -32.96115380933862582, 102.9999999999999858 ) ) ;
#2783 = CARTESIAN_POINT ( 'NONE',  ( 232.5999999999999375, -31.71562499938547930, -53.18285161636690361 ) ) ;
#2784 =( BOUNDED_CURVE ( )  B_SPLINE_CURVE ( 2, ( #7473, #16463, #11676, #7184, #11581, #4255, #17544, #10214, #2787 ),
 .UNSPECIFIED., .F., .F. ) 
 B_SPLINE_CURVE_WITH_KNOTS ( ( 3, 2, 2, 2, 3 ),
 ( 0.06250000000000002776, 0.06944444444444444753, 0.08333333333333332871, 0.09722222222222222376, 0.1041666666666666713 ),
 .UNSPECIFIED. ) 
 CURVE ( )  GEOMETRIC_REPRESENTATION_ITEM ( )  RATIONAL_B_SPLINE_CURVE ( ( 0.9330127018922194093, 0.9330127018922196314, 1.000000000000000000, 0.8660254037844387076, 1.000000000000000000, 0.8660254037844387076, 1.000000000000000000, 0.9330127018922192983, 0.9330127018922194093 ) ) 
 REPRESENTATION_ITEM ( '' )  );
#2785 = CARTESIAN_POINT ( 'NONE',  ( -85.15643035624999868, -32.35312499938549280, 101.5914258081833879 ) ) ;
#2786 = ORIENTED_EDGE ( 'NONE', *, *, #5809, .F. ) ;
#2787 = CARTESIAN_POINT ( 'NONE',  ( -82.40000000000000568, -30.56250000000001066, 96.99999999999998579 ) ) ;
#2788 = EDGE_CURVE ( 'NONE', #18284, #16539, #8118, .T. ) ;
#2789 = ADVANCED_FACE ( 'NONE', ( #9287 ), #15444, .T. ) ;
#2790 = CARTESIAN_POINT ( 'NONE',  ( 4.050480423730738799, 1.376911654797410955, -3.567926555162023394 ) ) ;
#2791 = LINE ( 'NONE', #14501, #4873 ) ;
#2792 = CARTESIAN_POINT ( 'NONE',  ( -83.90000000000000568, -31.72106250001229810, 102.5980762113533018 ) ) ;
#2793 = CARTESIAN_POINT ( 'NONE',  ( 3.861362476283255685, 2.629030857715988656, -3.671615880910370500 ) ) ;
#2794 = CARTESIAN_POINT ( 'NONE',  ( 233.9825576637931022, -32.00000000000000000, -47.41649131116869853 ) ) ;
#2795 = CARTESIAN_POINT ( 'NONE',  ( -79.64356964374999848, -30.81562499938548427, 99.99999999999998579 ) ) ;
#2796 = CARTESIAN_POINT ( 'NONE',  ( 232.5999999999999375, -33.93749999999999289, -47.00000000000011369 ) ) ;
#2797 = CARTESIAN_POINT ( 'NONE',  ( 85.15643035624999868, -32.99062499938548854, 101.5914258081833879 ) ) ;
#2798 = EDGE_CURVE ( 'NONE', #7197, #1583, #16448, .T. ) ;
#2799 = DIRECTION ( 'NONE',  ( 0.000000000000000000, 0.000000000000000000, 1.000000000000000000 ) ) ;
#2800 = CARTESIAN_POINT ( 'NONE',  ( 229.5999999999999375, -34.93124999877095860, 98.26794919243111792 ) ) ;
#2801 = CARTESIAN_POINT ( 'NONE',  ( 79.64356964374999848, -33.62812499938548427, -99.99999999999998579 ) ) ;
#2802 = CARTESIAN_POINT ( 'NONE',  ( -79.64356964375001269, -30.89062499938548711, -101.5914258081833879 ) ) ;
#2803 = ORIENTED_EDGE ( 'NONE', *, *, #8175, .F. ) ;
#2804 = CARTESIAN_POINT ( 'NONE',  ( 85.40000000000000568, -32.64374999877097139, 99.99999999999998579 ) ) ;
#2805 = CYLINDRICAL_SURFACE ( 'NONE', #4619, 5.199999999999996625 ) ;
#2806 = CARTESIAN_POINT ( 'NONE',  ( 233.9782151781249411, -34.45312499938548001, -52.38713871227520968 ) ) ;
#2807 = CARTESIAN_POINT ( 'NONE',  ( 235.5999999999999943, -34.25624999877096144, 101.7320508075688537 ) ) ;
#2808 = CARTESIAN_POINT ( 'NONE',  ( 4.000000000000000000, 2.309401076758497151, -5.000000000000000000 ) ) ;
#2809 = ORIENTED_EDGE ( 'NONE', *, *, #14777, .T. ) ;
#2810 = CARTESIAN_POINT ( 'NONE',  ( -82.39999999999999147, -34.97812499938547859, -96.81714838363319586 ) ) ;
#2811 = CARTESIAN_POINT ( 'NONE',  ( 4.000000000000000000, 0.8378280264232961239, -3.220590601395640018 ) ) ;
#2812 = VERTEX_POINT ( 'NONE', #4814 ) ;
#2813 = PLANE ( 'NONE',  #11708 ) ;
#2814 = CARTESIAN_POINT ( 'NONE',  ( -83.77821517812500929, -34.37812499938548427, -102.3871387122750889 ) ) ;
#2815 = CARTESIAN_POINT ( 'NONE',  ( 231.7961524227065695, -34.59240381056765301, -53.00000000000011369 ) ) ;
#2816 = CARTESIAN_POINT ( 'NONE',  ( -80.90000000000000568, -30.99374999877096926, -102.5980762113533018 ) ) ;
#2817 = CARTESIAN_POINT ( 'NONE',  ( 231.2217848218749339, -31.22812499938547859, 97.61286128772489690 ) ) ;
#2818 = CARTESIAN_POINT ( 'NONE',  ( -83.90000000000000568, -33.46874999877096712, 102.5980762113533018 ) ) ;
#2819 = CARTESIAN_POINT ( 'NONE',  ( -85.15643035624999868, -34.34062499938548285, 98.40857419181659793 ) ) ;
#2820 = CARTESIAN_POINT ( 'NONE',  ( 234.0999999999999375, -33.84374999877096002, 102.5980762113533018 ) ) ;
#2821 = CARTESIAN_POINT ( 'NONE',  ( -1.788378118793200470E-29, -3.597944987211158634E-13, -100.0000000000001137 ) ) ;
#2822 = CARTESIAN_POINT ( 'NONE',  ( 232.5999999999999375, -33.43124999877096570, 102.9999999999999858 ) ) ;
#2823 = CARTESIAN_POINT ( 'NONE',  ( 80.90000000000000568, -31.44374999877096855, -97.40192378864668399 ) ) ;
#2824 = CARTESIAN_POINT ( 'NONE',  ( 234.0999999999999375, -34.19999999999999574, 97.40192378864668399 ) ) ;
#2825 = B_SPLINE_CURVE_WITH_KNOTS ( 'NONE', 3,
 ( #8703, #8412, #5597, #17312, #11542, #17694 ),
 .UNSPECIFIED., .F., .F.,
 ( 4, 2, 4 ),
 ( 0.005852013098461907557, 0.006875955139453160392, 0.007899897180444414094 ),
 .UNSPECIFIED. ) ;
#2826 = VERTEX_POINT ( 'NONE', #1869 ) ;
#2827 = CARTESIAN_POINT ( 'NONE',  ( 79.64356964374998427, -34.45312499938548711, -101.5914258081833879 ) ) ;
#2828 = EDGE_CURVE ( 'NONE', #14354, #11020, #7827, .T. ) ;
#2829 = CARTESIAN_POINT ( 'NONE',  ( 234.0999999999999375, -31.89374999877096073, 97.40192378864668399 ) ) ;
#2830 = CARTESIAN_POINT ( 'NONE',  ( 235.5999999999999943, -33.28124999877096002, -51.73205080756900287 ) ) ;
#2831 = CARTESIAN_POINT ( 'NONE',  ( -85.15643035625001289, -34.22812499938548569, 98.40857419181659793 ) ) ;
#2832 = VERTEX_POINT ( 'NONE', #12322 ) ;
#2833 = ORIENTED_EDGE ( 'NONE', *, *, #4119, .T. ) ;
#2834 = CARTESIAN_POINT ( 'NONE',  ( -4.197393957002303999, -7.773935952363655451E-14, -3.503767560748929810 ) ) ;
#2835 = CARTESIAN_POINT ( 'NONE',  ( 4.207491450040567571, -2.029819825146485179, -3.671670828759567407 ) ) ;
#2836 = ORIENTED_EDGE ( 'NONE', *, *, #10425, .F. ) ;
#2837 = CARTESIAN_POINT ( 'NONE',  ( -80.52691934816500918, -34.99999999999999289, 102.0537355158133010 ) ) ;
#2838 = CARTESIAN_POINT ( 'NONE',  ( 85.40000000000000568, -34.50000000000000000, -99.99999999999998579 ) ) ;
#2839 = CARTESIAN_POINT ( 'NONE',  ( 113.0000000000000000, 10.19999999999997264, -139.9999999999999716 ) ) ;
#2840 = CARTESIAN_POINT ( 'NONE',  ( -79.64356964375001269, -34.11562499938548854, 101.5914258081833879 ) ) ;
#2841 = CARTESIAN_POINT ( 'NONE',  ( -85.40000000000000568, -31.83750000000000568, 98.26794919243111792 ) ) ;
#2842 = CARTESIAN_POINT ( 'NONE',  ( 233.9419434205216817, -35.00000000000000711, -52.61493892574790010 ) ) ;
#2843 = CARTESIAN_POINT ( 'NONE',  ( 232.1470656674052577, -31.99999999999997868, -52.80109480795715626 ) ) ;
#2844 = EDGE_CURVE ( 'NONE', #4900, #13568, #11392, .T. ) ;
#2845 =( REPRESENTATION_RELATIONSHIP ('NONE','NONE', #14468, #14995 ) REPRESENTATION_RELATIONSHIP_WITH_TRANSFORMATION ( #18358 )SHAPE_REPRESENTATION_RELATIONSHIP( ) );
#2846 = CARTESIAN_POINT ( 'NONE',  ( -84.69814099439363986, -35.09873396208577390, 98.07164630581206666 ) ) ;
#2847 = CARTESIAN_POINT ( 'NONE',  ( 85.24876232368478668, -35.00000000000000711, 99.45334139304991083 ) ) ;
#2848 = DIRECTION ( 'NONE',  ( 1.000000000000000000, -0.000000000000000000, -2.407412430484046130E-31 ) ) ;
#2849 = VERTEX_POINT ( 'NONE', #10066 ) ;
#2850 =( NAMED_UNIT ( * ) SI_UNIT ( $, .STERADIAN. ) SOLID_ANGLE_UNIT ( ) );
#2851 = CARTESIAN_POINT ( 'NONE',  ( -85.15643035624999868, -31.00312499938548072, -98.40857419181659793 ) ) ;
#2852 = CYLINDRICAL_SURFACE ( 'NONE', #16778, 3.000000000000002665 ) ;
#2853 = DIRECTION ( 'NONE',  ( -0.000000000000000000, -1.000000000000000000, -0.000000000000000000 ) ) ;
#2854 = DIRECTION ( 'NONE',  ( 1.000000000000000000, -1.586032892321652285E-15, 0.000000000000000000 ) ) ;
#2855 = CARTESIAN_POINT ( 'NONE',  ( -81.02178482187500208, -35.05312499938548854, 102.3871387122750889 ) ) ;
#2856 = CARTESIAN_POINT ( 'NONE',  ( 79.39999999999999147, -33.33749999999999858, 101.7320508075688963 ) ) ;
#2857 = CARTESIAN_POINT ( 'NONE',  ( 233.9782151781249411, -34.04062499938547859, -47.61286128772501769 ) ) ;
#2858 = ORIENTED_EDGE ( 'NONE', *, *, #101, .F. ) ;
#2859 = ORIENTED_EDGE ( 'NONE', *, *, #9611, .T. ) ;
#2860 = CARTESIAN_POINT ( 'NONE',  ( -84.01447415327271528, -35.02670941564510088, -102.7431224211893692 ) ) ;
#2861 = CARTESIAN_POINT ( 'NONE',  ( -80.90000000000000568, -32.10000000000000142, 102.5980762113533018 ) ) ;
#2862 = CARTESIAN_POINT ( 'NONE',  ( -85.40000000000000568, -31.25624999877096855, 101.7320508075688679 ) ) ;
#2863 = CARTESIAN_POINT ( 'NONE',  ( 85.40000000000000568, -30.41249999999999787, 98.26794919243111792 ) ) ;
#2864 = CARTESIAN_POINT ( 'NONE',  ( 102.9999999999999858, -29.80000000000000071, -100.0000000000000000 ) ) ;
#2865 = CARTESIAN_POINT ( 'NONE',  ( 232.5999999999999375, -31.15312499938547930, 96.81714838363319586 ) ) ;
#2866 = CARTESIAN_POINT ( 'NONE',  ( 235.3564303562499447, -34.00312499938547717, -48.40857419181671162 ) ) ;
#2867 = CARTESIAN_POINT ( 'NONE',  ( 81.02178482187500208, -34.04062499938548569, 97.61286128772489690 ) ) ;
#2868 = AXIS2_PLACEMENT_3D ( 'NONE', #18269, #13954, #9665 ) ;
#2869 = AXIS2_PLACEMENT_3D ( 'NONE', #5103, #11045, #17011 ) ;
#2870 = CARTESIAN_POINT ( 'NONE',  ( 81.02178482187500208, -31.79062499938548925, -102.3871387122750889 ) ) ;
#2871 = CARTESIAN_POINT ( 'NONE',  ( 231.2217848218749339, -34.71562499938547575, -52.38713871227520968 ) ) ;
#2872 = FACE_OUTER_BOUND ( 'NONE', #12974, .T. ) ;
#2873 = CARTESIAN_POINT ( 'NONE',  ( 81.02178482187500208, -32.54062499938548569, -97.61286128772489690 ) ) ;
#2874 = VERTEX_POINT ( 'NONE', #4199 ) ;
#2875 = LINE ( 'NONE', #6004, #5398 ) ;
#2876 = DIRECTION ( 'NONE',  ( -0.000000000000000000, -1.000000000000000000, -0.000000000000000000 ) ) ;
#2877 = CARTESIAN_POINT ( 'NONE',  ( 231.2217848218749339, -30.62812499938548072, -47.61286128772501769 ) ) ;
#2878 = CARTESIAN_POINT ( 'NONE',  ( -85.15643035624999868, -32.80312499938548854, 101.5914258081833879 ) ) ;
#2879 = VERTEX_POINT ( 'NONE', #6858 ) ;
#2880 = CARTESIAN_POINT ( 'NONE',  ( -85.40000000000000568, -33.99374999877097281, 99.99999999999998579 ) ) ;
#2881 = VECTOR ( 'NONE', #3509, 1000.000000000000000 ) ;
#2882 = AXIS2_PLACEMENT_3D ( 'NONE', #7560, #352, #1699 ) ;
#2883 = CARTESIAN_POINT ( 'NONE',  ( 235.3564303562499447, -32.65312499938547575, 101.5914258081833879 ) ) ;
#2884 = DIRECTION ( 'NONE',  ( 0.000000000000000000, 0.000000000000000000, 1.000000000000000000 ) ) ;
#2885 = CARTESIAN_POINT ( 'NONE',  ( -82.39999999999999147, -32.58356250001229881, 103.4641016151377499 ) ) ;
#2886 = LINE ( 'NONE', #14698, #15152 ) ;
#2887 = DIRECTION ( 'NONE',  ( -0.000000000000000000, -0.000000000000000000, -1.000000000000000000 ) ) ;
#2888 = CARTESIAN_POINT ( 'NONE',  ( -83.77821517812500929, -30.96562499938548640, 102.3871387122750889 ) ) ;
#2889 = CARTESIAN_POINT ( 'NONE',  ( 229.7688980899111186, -34.99999999999998579, 99.14248198115953414 ) ) ;
#2890 = CARTESIAN_POINT ( 'NONE',  ( 83.77821517812500929, -33.32812499938548711, 97.61286128772489690 ) ) ;
#2891 = CARTESIAN_POINT ( 'NONE',  ( 82.40000000000000568, -30.00000000000000355, 99.99999999999998579 ) ) ;
#2892 = CARTESIAN_POINT ( 'NONE',  ( -79.39999999999999147, -32.51250000000000284, -98.26794919243113213 ) ) ;
#2893 = CARTESIAN_POINT ( 'NONE',  ( -85.11512745526623291, -32.00000000000000000, -99.40473233008064824 ) ) ;
#2894 = CARTESIAN_POINT ( 'NONE',  ( -79.64356964375001269, -31.79062499938548569, -101.5914258081833879 ) ) ;
#2895 = CIRCLE ( 'NONE', #10702, 2.055000000000000160 ) ;
#2896 =( BOUNDED_CURVE ( )  B_SPLINE_CURVE ( 2, ( #13460, #96, #16591, #16499, #6048, #3101, #2820, #9060, #3196 ),
 .UNSPECIFIED., .F., .F. ) 
 B_SPLINE_CURVE_WITH_KNOTS ( ( 3, 2, 2, 2, 3 ),
 ( 0.6041666666666667407, 0.6111111111111111605, 0.6250000000000000000, 0.6388888888888888395, 0.6458333333333331483 ),
 .UNSPECIFIED. ) 
 CURVE ( )  GEOMETRIC_REPRESENTATION_ITEM ( )  RATIONAL_B_SPLINE_CURVE ( ( 0.9330127018922192983, 0.9330127018922198534, 1.000000000000000000, 0.8660254037844387076, 1.000000000000000000, 0.8660254037844387076, 1.000000000000000000, 0.9330127018922209636, 0.9330127018922194093 ) ) 
 REPRESENTATION_ITEM ( '' )  );
#2897 = ORIENTED_EDGE ( 'NONE', *, *, #14345, .T. ) ;
#2898 = CARTESIAN_POINT ( 'NONE',  ( 83.90000000000000568, -32.71874999877096712, 102.5980762113533018 ) ) ;
#2899 = CYLINDRICAL_SURFACE ( 'NONE', #8645, 3.000000000000002665 ) ;
#2900 = CARTESIAN_POINT ( 'NONE',  ( 229.8435696437499303, -34.75312499938547717, -50.00000000000011369 ) ) ;
#2901 = CARTESIAN_POINT ( 'NONE',  ( -85.15643035624999868, -30.66562499938548569, 101.5914258081833879 ) ) ;
#2902 = CARTESIAN_POINT ( 'NONE',  ( 82.14831453752277923, -31.99999999999999289, 102.8584433575407218 ) ) ;
#2903 = ORIENTED_EDGE ( 'NONE', *, *, #12958, .F. ) ;
#2904 = CARTESIAN_POINT ( 'NONE',  ( -83.77821517812500929, -33.81562499938548427, -102.3871387122750889 ) ) ;
#2905 = CARTESIAN_POINT ( 'NONE',  ( -99.99999999999998579, -3.000000000000000000, 150.0000000000000000 ) ) ;
#2906 = EDGE_CURVE ( 'NONE', #18744, #9588, #16025, .T. ) ;
#2907 = CARTESIAN_POINT ( 'NONE',  ( -79.39999999999999147, -30.26250000000000284, 101.7320508075688537 ) ) ;
#2908 = CARTESIAN_POINT ( 'NONE',  ( -83.77821517812500929, -33.77812499938548285, -97.61286128772489690 ) ) ;
#2909 = CIRCLE ( 'NONE', #13819, 6.000000000000005329 ) ;
#2910 = CARTESIAN_POINT ( 'NONE',  ( 231.0999999999999375, -34.57499999999999574, -52.59807621135342970 ) ) ;
#2911 = CARTESIAN_POINT ( 'NONE',  ( -83.90000000000000568, -31.81874999877096855, -102.5980762113533018 ) ) ;
#2912 = CARTESIAN_POINT ( 'NONE',  ( 233.9782151781249411, -32.65312499938548285, 97.61286128772489690 ) ) ;
#2913 = CARTESIAN_POINT ( 'NONE',  ( -85.40000000000000568, -32.61018749875868394, 101.7320508075688679 ) ) ;
#2914 = CARTESIAN_POINT ( 'NONE',  ( -79.64356964375001269, -32.76562499938548711, 101.5914258081833879 ) ) ;
#2915 = CARTESIAN_POINT ( 'NONE',  ( -82.39999999999999147, -34.75312499938548427, -103.1828516163667899 ) ) ;
#2916 = CARTESIAN_POINT ( 'NONE',  ( -82.40000000000001990, -32.53124999877097423, 103.0000000000000000 ) ) ;
#2917 = EDGE_CURVE ( 'NONE', #19255, #5568, #6165, .T. ) ;
#2918 = CARTESIAN_POINT ( 'NONE',  ( 80.90000000000000568, -32.94374999877096855, -102.5980762113533018 ) ) ;
#2919 = CARTESIAN_POINT ( 'NONE',  ( 231.0999999999999375, -34.12499999999999289, 97.40192378864668399 ) ) ;
#2920 = EDGE_CURVE ( 'NONE', #3185, #19282, #10647, .T. ) ;
#2921 = ORIENTED_EDGE ( 'NONE', *, *, #8685, .T. ) ;
#2922 = CARTESIAN_POINT ( 'NONE',  ( 2.500000000000000444, 0.000000000000000000, -25.03750572909317285 ) ) ;
#2923 = CARTESIAN_POINT ( 'NONE',  ( 232.5999999999999375, -30.36562499938548498, 96.81714838363319586 ) ) ;
#2924 = CARTESIAN_POINT ( 'NONE',  ( 234.0999999999999375, -34.59374999877096002, -52.59807621135342970 ) ) ;
#2925 = ADVANCED_FACE ( 'NONE', ( #7136 ), #5679, .F. ) ;
#2926 = CARTESIAN_POINT ( 'NONE',  ( -79.64356964374999848, -33.96562499938548285, 99.99999999999998579 ) ) ;
#2927 = ORIENTED_EDGE ( 'NONE', *, *, #6057, .F. ) ;
#2928 = ORIENTED_EDGE ( 'NONE', *, *, #10234, .F. ) ;
#2929 = CARTESIAN_POINT ( 'NONE',  ( 82.40000000000000568, -34.38749999999999574, -102.9999999999999858 ) ) ;
#2930 = DIRECTION ( 'NONE',  ( 2.312964634635736745E-15, 1.000000000000000000, 0.000000000000000000 ) ) ;
#2931 = DIRECTION ( 'NONE',  ( 0.000000000000000000, -1.000000000000000000, 0.000000000000000000 ) ) ;
#2932 = ORIENTED_EDGE ( 'NONE', *, *, #3342, .F. ) ;
#2933 = CARTESIAN_POINT ( 'NONE',  ( -81.44948931429647132, -34.99999999999999289, 102.5934467159354284 ) ) ;
#2934 = DIRECTION ( 'NONE',  ( 1.000000000000000000, -1.387778780781445676E-15, -2.407412430484046130E-31 ) ) ;
#2935 = CARTESIAN_POINT ( 'NONE',  ( -79.64356964375001269, -33.59062499938548285, 98.40857419181659793 ) ) ;
#2936 = CARTESIAN_POINT ( 'NONE',  ( -82.39999999999999147, -33.71249999999999858, 96.53589838486223584 ) ) ;
#2937 = EDGE_CURVE ( 'NONE', #3433, #6642, #16534, .T. ) ;
#2938 = CARTESIAN_POINT ( 'NONE',  ( -80.90000000000000568, -30.99374999877096926, 97.40192378864668399 ) ) ;
#2939 = CARTESIAN_POINT ( 'NONE',  ( -82.40000000000000568, -30.00000000000000355, 99.99999999999998579 ) ) ;
#2940 = CARTESIAN_POINT ( 'NONE',  ( 4.086262629614028086, 1.979770830881088850, 3.570936333571100629 ) ) ;
#2941 = CARTESIAN_POINT ( 'NONE',  ( -79.91954014136211981, -34.99999999999999289, -101.4427624130898238 ) ) ;
#2942 = CARTESIAN_POINT ( 'NONE',  ( 235.3564303562499447, -30.36562499938547788, 99.99999999999998579 ) ) ;
#2943 = ORIENTED_EDGE ( 'NONE', *, *, #13179, .F. ) ;
#2944 = CARTESIAN_POINT ( 'NONE',  ( -85.15643035624999868, -33.77812499938548285, -101.5914258081833879 ) ) ;
#2945 = CARTESIAN_POINT ( 'NONE',  ( -85.40000000000000568, -33.63750000000000284, 98.26794919243111792 ) ) ;
#2946 = CARTESIAN_POINT ( 'NONE',  ( -84.51155386534844638, -35.25364837475780888, 98.22820752270799005 ) ) ;
#2947 = CARTESIAN_POINT ( 'NONE',  ( 229.5999999999999375, -34.48124999877096286, 98.26794919243111792 ) ) ;
#2948 = CARTESIAN_POINT ( 'NONE',  ( -79.64356964374999848, -32.16562499938548569, 99.99999999999998579 ) ) ;
#2949 = LINE ( 'NONE', #5893, #17854 ) ;
#2950 = EDGE_CURVE ( 'NONE', #3433, #6725, #4244, .T. ) ;
#2951 = CARTESIAN_POINT ( 'NONE',  ( 229.8435696437499871, -32.80312499938548143, -48.40857419181671162 ) ) ;
#2952 = ORIENTED_EDGE ( 'NONE', *, *, #9274, .F. ) ;
#2953 = ORIENTED_EDGE ( 'NONE', *, *, #1112, .F. ) ;
#2954 = CARTESIAN_POINT ( 'NONE',  ( -85.16931825408420309, -31.99999999999999289, 100.2387112178438144 ) ) ;
#2955 = CARTESIAN_POINT ( 'NONE',  ( -83.90000000000000568, -30.97500000000000142, 97.40192378864668399 ) ) ;
#2956 = CARTESIAN_POINT ( 'NONE',  ( -85.40000000000000568, -32.19374999877096855, 99.99999999999998579 ) ) ;
#2957 = CARTESIAN_POINT ( 'NONE',  ( 79.39999999999999147, -31.16250000000000497, 98.26794919243113213 ) ) ;
#2958 = EDGE_CURVE ( 'NONE', #11282, #609, #5302, .T. ) ;
#2959 = PLANE ( 'NONE',  #16788 ) ;
#2960 = CARTESIAN_POINT ( 'NONE',  ( 235.3564303562499447, -33.02812499938547575, 98.40857419181659793 ) ) ;
#2961 = CARTESIAN_POINT ( 'NONE',  ( 233.9782151781249411, -33.44062499938547717, -52.38713871227520968 ) ) ;
#2962 = CARTESIAN_POINT ( 'NONE',  ( 85.15643035625001289, -33.74062499938548854, 99.99999999999998579 ) ) ;
#2963 = CARTESIAN_POINT ( 'NONE',  ( 83.77821517812500929, -30.66562499938548569, -97.61286128772489690 ) ) ;
#2964 = ORIENTED_EDGE ( 'NONE', *, *, #6872, .F. ) ;
#2965 = CARTESIAN_POINT ( 'NONE',  ( 235.5999999999999375, -30.22499999999999432, -50.00000000000011369 ) ) ;
#2966 = CARTESIAN_POINT ( 'NONE',  ( 79.39999999999999147, -34.25624999877096855, 98.26794919243113213 ) ) ;
#2967 = CARTESIAN_POINT ( 'NONE',  ( 79.64356964375001269, -33.10312499938549280, -101.5914258081833879 ) ) ;
#2968 = VERTEX_POINT ( 'NONE', #4663 ) ;
#2969 = CARTESIAN_POINT ( 'NONE',  ( 232.5999999999999375, -32.98124999877095576, 102.9999999999999858 ) ) ;
#2970 = CARTESIAN_POINT ( 'NONE',  ( -85.40000000000000568, -34.93124999877096570, 98.26794919243111792 ) ) ;
#2971 = CARTESIAN_POINT ( 'NONE',  ( 233.9782151781249411, -31.00312499938548072, -47.61286128772501769 ) ) ;
#2972 = CARTESIAN_POINT ( 'NONE',  ( -81.02178482187500208, -34.94062499938548427, 102.3871387122750889 ) ) ;
#2973 = ORIENTED_EDGE ( 'NONE', *, *, #16055, .F. ) ;
#2974 = CARTESIAN_POINT ( 'NONE',  ( 244.7999999999999545, -29.80000000000002203, -100.0000000000000142 ) ) ;
#2975 = CARTESIAN_POINT ( 'NONE',  ( 235.3564303562499447, -34.90312499938547575, 101.5914258081833879 ) ) ;
#2976 = CARTESIAN_POINT ( 'NONE',  ( 83.77821517812500929, -30.21562499938548285, 102.3871387122750889 ) ) ;
#2977 = CARTESIAN_POINT ( 'NONE',  ( -79.39999999999999147, -32.47106250001229455, 99.99999999999998579 ) ) ;
#2978 = CARTESIAN_POINT ( 'NONE',  ( 0.2174200650117588118, -3.876582599186217948, -0.2855619784720692111 ) ) ;
#2979 = LINE ( 'NONE', #10504, #7735 ) ;
#2980 = CARTESIAN_POINT ( 'NONE',  ( -83.77821517812500929, -32.46562499938548285, 97.61286128772489690 ) ) ;
#2981 = DIRECTION ( 'NONE',  ( 0.000000000000000000, 0.000000000000000000, 1.000000000000000000 ) ) ;
#2982 = CARTESIAN_POINT ( 'NONE',  ( 81.02178482187500208, -32.65312499938548996, 102.3871387122750889 ) ) ;
#2983 = CARTESIAN_POINT ( 'NONE',  ( 80.90000000000000568, -32.04374999877096997, 97.40192378864668399 ) ) ;
#2984 = CARTESIAN_POINT ( 'NONE',  ( 229.5999999999999375, -34.85624999877096286, 101.7320508075688821 ) ) ;
#2985 = CARTESIAN_POINT ( 'NONE',  ( -81.02178482187500208, -32.80312499938548854, 102.3871387122750889 ) ) ;
#2986 = CARTESIAN_POINT ( 'NONE',  ( -79.64356964375001269, -32.31562499938548427, -98.40857419181659793 ) ) ;
#2987 = VECTOR ( 'NONE', #16966, 1000.000000000000000 ) ;
#2988 = VERTEX_POINT ( 'NONE', #9141 ) ;
#2989 = CARTESIAN_POINT ( 'NONE',  ( 85.40000000000000568, -34.93124999877096570, 101.7320508075688679 ) ) ;
#2990 = CARTESIAN_POINT ( 'NONE',  ( -1.655952806101422814, 3.662737355149034979, -7.623296525288699970E-18 ) ) ;
#2991 = CARTESIAN_POINT ( 'NONE',  ( 229.8435696437499871, -35.22676544108146857, -51.00325357418267913 ) ) ;
#2992 = CARTESIAN_POINT ( 'NONE',  ( 82.39999999999999147, -32.36250000000000426, -96.99999999999998579 ) ) ;
#2993 = CARTESIAN_POINT ( 'NONE',  ( -81.02178482187500208, -31.45312499938549067, 102.3871387122750889 ) ) ;
#2994 = CARTESIAN_POINT ( 'NONE',  ( 82.40000000000001990, -33.88124999877096855, -103.0000000000000000 ) ) ;
#2995 = ORIENTED_EDGE ( 'NONE', *, *, #5185, .F. ) ;
#2996 = CARTESIAN_POINT ( 'NONE',  ( -80.90000000000000568, -31.50000000000000000, -102.5980762113533018 ) ) ;
#2997 = CARTESIAN_POINT ( 'NONE',  ( 4.180232103119976728, 2.085387772176679366, -3.570466442734698820 ) ) ;
#2998 = DIRECTION ( 'NONE',  ( 0.000000000000000000, 1.000000000000000000, 0.000000000000000000 ) ) ;
#2999 = CARTESIAN_POINT ( 'NONE',  ( -85.15643035624999868, -33.36562499938548854, -98.40857419181659793 ) ) ;
#3000 = CIRCLE ( 'NONE', #6122, 2.500000000000000888 ) ;
#3001 = CARTESIAN_POINT ( 'NONE',  ( 229.5999999999999375, -34.53749999999999432, -51.73205080756898866 ) ) ;
#3002 = CARTESIAN_POINT ( 'NONE',  ( -85.40000000000000568, -30.84374999877096712, -99.99999999999998579 ) ) ;
#3003 = CARTESIAN_POINT ( 'NONE',  ( 232.5999999999999375, -31.94062499938548072, 103.1828516163667899 ) ) ;
#3004 = CARTESIAN_POINT ( 'NONE',  ( -83.90000000000000568, -31.67268749875867684, 102.5980762113533018 ) ) ;
#3005 = CARTESIAN_POINT ( 'NONE',  ( -85.15643035624999868, -32.54062499938548569, 98.40857419181659793 ) ) ;
#3006 = CARTESIAN_POINT ( 'NONE',  ( -79.39999999999999147, -31.57499999999999929, 99.99999999999998579 ) ) ;
#3007 = CARTESIAN_POINT ( 'NONE',  ( 81.02178482187500208, -33.59062499938548285, 97.61286128772489690 ) ) ;
#3008 = CARTESIAN_POINT ( 'NONE',  ( 79.39999999999999147, -32.43750000000000000, -98.26794919243110371 ) ) ;
#3009 = LINE ( 'NONE', #295, #13323 ) ;
#3010 = CARTESIAN_POINT ( 'NONE',  ( 79.39999999999999147, -35.11874999877096570, -99.99999999999998579 ) ) ;
#3011 = CARTESIAN_POINT ( 'NONE',  ( 234.0999999999999375, -32.84999999999999432, 97.40192378864668399 ) ) ;
#3012 = EDGE_CURVE ( 'NONE', #9387, #104, #4737, .T. ) ;
#3013 = ADVANCED_FACE ( 'NONE', ( #16671 ), #11981, .T. ) ;
#3014 = ORIENTED_EDGE ( 'NONE', *, *, #14640, .F. ) ;
#3015 = CARTESIAN_POINT ( 'NONE',  ( 229.8435696437499587, -32.91562499938547859, -48.40857419181671162 ) ) ;
#3016 = CARTESIAN_POINT ( 'NONE',  ( 235.5999999999999943, -35.08124999877096428, 98.26794919243110371 ) ) ;
#3017 = CARTESIAN_POINT ( 'NONE',  ( 235.5999999999999375, -32.41874999877096286, -50.00000000000011369 ) ) ;
#3018 = CARTESIAN_POINT ( 'NONE',  ( -81.02178482187500208, -33.14062499938548711, 102.3871387122750889 ) ) ;
#3019 = VERTEX_POINT ( 'NONE', #81 ) ;
#3020 = VERTEX_POINT ( 'NONE', #3087 ) ;
#3021 = CARTESIAN_POINT ( 'NONE',  ( 111.0000000000000142, 15.19999999999997797, -136.6833752096445380 ) ) ;
#3022 = DIRECTION ( 'NONE',  ( 0.000000000000000000, -1.000000000000000000, 0.000000000000000000 ) ) ;
#3023 = CARTESIAN_POINT ( 'NONE',  ( -83.90000000000000568, -32.26874999877097139, 97.40192378864668399 ) ) ;
#3024 = ORIENTED_EDGE ( 'NONE', *, *, #18429, .T. ) ;
#3025 = LINE ( 'NONE', #1574, #12339 ) ;
#3026 = MECHANICAL_DESIGN_GEOMETRIC_PRESENTATION_REPRESENTATION (  '', ( #8945 ), #15212 ) ;
#3027 = FACE_OUTER_BOUND ( 'NONE', #11912, .T. ) ;
#3028 = EDGE_CURVE ( 'NONE', #14891, #19060, #15384, .T. ) ;
#3029 = CARTESIAN_POINT ( 'NONE',  ( -85.15643035624999868, -32.99062499938548854, 98.40857419181659793 ) ) ;
#3030 = CARTESIAN_POINT ( 'NONE',  ( -79.39999999999999147, -34.72500000000000142, 99.99999999999998579 ) ) ;
#3031 = EDGE_CURVE ( 'NONE', #6366, #14034, #13631, .T. ) ;
#3032 = CARTESIAN_POINT ( 'NONE',  ( -79.39999999999999147, -31.03124999877097068, 98.26794919243110371 ) ) ;
#3033 = DIRECTION ( 'NONE',  ( -1.000000000000000000, 0.000000000000000000, 0.000000000000000000 ) ) ;
#3034 = CARTESIAN_POINT ( 'NONE',  ( 82.40000000000000568, -30.00000000000000355, 99.99999999999998579 ) ) ;
#3035 = CARTESIAN_POINT ( 'NONE',  ( 0.000000000000000000, 0.000000000000000000, 0.000000000000000000 ) ) ;
#3036 = CARTESIAN_POINT ( 'NONE',  ( 104.5000000000000142, 12.69999999999998508, 112.0000000000000142 ) ) ;
#3037 = CARTESIAN_POINT ( 'NONE',  ( -83.90000000000000568, -34.42500000000000426, -97.40192378864668399 ) ) ;
#3038 = ORIENTED_EDGE ( 'NONE', *, *, #3467, .F. ) ;
#3039 = VECTOR ( 'NONE', #11839, 1000.000000000000000 ) ;
#3040 = CARTESIAN_POINT ( 'NONE',  ( -82.39999999999999147, -32.72812499938548569, -96.81714838363319586 ) ) ;
#3041 = CARTESIAN_POINT ( 'NONE',  ( 109.9999999999999432, -29.80000000000003268, -130.0000000000000000 ) ) ;
#3042 = CARTESIAN_POINT ( 'NONE',  ( 2.682243648011666703, 3.070208061305304881, -0.04852650426601266831 ) ) ;
#3043 = CARTESIAN_POINT ( 'NONE',  ( 81.44948931429642869, -35.00000000000001421, -102.5934467159354284 ) ) ;
#3044 = CARTESIAN_POINT ( 'NONE',  ( -79.64356964374999848, -31.71562499938548285, 99.99999999999998579 ) ) ;
#3045 = CARTESIAN_POINT ( 'NONE',  ( 82.40000000000001990, -32.13750000000000284, -103.0000000000000000 ) ) ;
#3046 = CARTESIAN_POINT ( 'NONE',  ( 231.2217848218749339, -32.01562499938548001, -52.38713871227520968 ) ) ;
#3047 = CIRCLE ( 'NONE', #12407, 5.200000000000009948 ) ;
#3048 = ORIENTED_EDGE ( 'NONE', *, *, #6746, .F. ) ;
#3049 = VERTEX_POINT ( 'NONE', #2992 ) ;
#3050 = CARTESIAN_POINT ( 'NONE',  ( -83.90000000000000568, -34.87500000000000000, -97.40192378864668399 ) ) ;
#3051 = CARTESIAN_POINT ( 'NONE',  ( -82.39999999999999147, -31.91250000000000497, 96.53589838486223584 ) ) ;
#3052 = CARTESIAN_POINT ( 'NONE',  ( -85.40000000000000568, -31.29374999877096997, 99.99999999999998579 ) ) ;
#3053 = CARTESIAN_POINT ( 'NONE',  ( 85.40000000000000568, -31.35000000000000142, 99.99999999999998579 ) ) ;
#3054 = AXIS2_PLACEMENT_3D ( 'NONE', #12607, #15347, #17107 ) ;
#3055 = CARTESIAN_POINT ( 'NONE',  ( -82.15584532983336885, -31.99999999999999289, -97.13032736203112449 ) ) ;
#3056 = CARTESIAN_POINT ( 'NONE',  ( 229.8435696437499871, -33.70312499938548001, 101.5914258081833879 ) ) ;
#3057 = CARTESIAN_POINT ( 'NONE',  ( 82.40000000000000568, -32.08124999877097139, 97.00000000000000000 ) ) ;
#3058 = CARTESIAN_POINT ( 'NONE',  ( -82.40000000000001990, -33.88124999877096855, 103.0000000000000000 ) ) ;
#3059 = CONICAL_SURFACE ( 'NONE', #8682, 4.000000000000000000, 0.8911886515913786111 ) ;
#3060 = CARTESIAN_POINT ( 'NONE',  ( 81.02178482187500208, -30.89062499938548711, -102.3871387122750889 ) ) ;
#3061 = ORIENTED_EDGE ( 'NONE', *, *, #14228, .F. ) ;
#3062 = CARTESIAN_POINT ( 'NONE',  ( 235.5999999999999375, -30.67499999999999361, -50.00000000000011369 ) ) ;
#3063 = CARTESIAN_POINT ( 'NONE',  ( 82.39999999999999147, -34.33124999877097139, 97.00000000000000000 ) ) ;
#3064 = CARTESIAN_POINT ( 'NONE',  ( 79.64356964374999848, -33.06562499938548427, -99.99999999999998579 ) ) ;
#3065 = LINE ( 'NONE', #5914, #6339 ) ;
#3066 = ADVANCED_FACE ( 'NONE', ( #1631 ), #4764, .F. ) ;
#3067 = CARTESIAN_POINT ( 'NONE',  ( -79.39999999999999147, -34.72500000000000142, 99.99999999999998579 ) ) ;
#3068 = CARTESIAN_POINT ( 'NONE',  ( -85.40000000000000568, -31.31250000000000000, 101.7320508075688679 ) ) ;
#3069 = ORIENTED_EDGE ( 'NONE', *, *, #12723, .F. ) ;
#3070 = CARTESIAN_POINT ( 'NONE',  ( -82.40000000000000568, -33.03750000000000142, 102.9999999999999858 ) ) ;
#3071 = AXIS2_PLACEMENT_3D ( 'NONE', #13290, #10083, #16040 ) ;
#3072 = CARTESIAN_POINT ( 'NONE',  ( 231.2217848218749339, -33.81562499938547717, 97.61286128772489690 ) ) ;
#3073 = CARTESIAN_POINT ( 'NONE',  ( -82.40000000000000568, -34.10624999877096997, 96.99999999999998579 ) ) ;
#3074 = CARTESIAN_POINT ( 'NONE',  ( -85.40000000000000568, -31.34606250001229810, 99.99999999999998579 ) ) ;
#3075 = CARTESIAN_POINT ( 'NONE',  ( 235.4117376914898898, -32.00000000000000000, -51.04600724388262023 ) ) ;
#3076 = CARTESIAN_POINT ( 'NONE',  ( -83.20384757729337366, -32.34240381056766722, 97.00000000000000000 ) ) ;
#3077 = CARTESIAN_POINT ( 'NONE',  ( -85.15643035624999868, -31.45312499938548356, 101.5914258081833879 ) ) ;
#3078 = CARTESIAN_POINT ( 'NONE',  ( 229.7064227204490408, -35.00000000000000711, 100.3154961327744985 ) ) ;
#3079 = CARTESIAN_POINT ( 'NONE',  ( 79.64356964375001269, -33.14062499938548711, 101.5914258081833879 ) ) ;
#3080 = CARTESIAN_POINT ( 'NONE',  ( 79.64356964375001269, -30.44062499938548783, -98.40857419181659793 ) ) ;
#3081 = CYLINDRICAL_SURFACE ( 'NONE', #17126, 2.649999999999985700 ) ;
#3082 = CARTESIAN_POINT ( 'NONE',  ( -82.39999999999999147, -32.39062499938548711, 103.1828516163667899 ) ) ;
#3083 = CARTESIAN_POINT ( 'NONE',  ( -79.64356964375001269, -30.96562499938548640, -98.40857419181659793 ) ) ;
#3084 = VERTEX_POINT ( 'NONE', #6227 ) ;
#3085 = CARTESIAN_POINT ( 'NONE',  ( 83.90000000000000568, -34.96874999877096712, 102.5980762113533018 ) ) ;
#3086 = DIRECTION ( 'NONE',  ( -4.970554372426382520E-17, -1.000000000000000000, 3.491481338843133355E-15 ) ) ;
#3087 = CARTESIAN_POINT ( 'NONE',  ( 4.071447262713888016, 4.041451884327382338, 0.000000000000000000 ) ) ;
#3088 = CARTESIAN_POINT ( 'NONE',  ( -85.15643035625001289, -32.50312499938548427, 99.99999999999998579 ) ) ;
#3089 = DIRECTION ( 'NONE',  ( -0.000000000000000000, -0.000000000000000000, -1.000000000000000000 ) ) ;
#3090 = EDGE_LOOP ( 'NONE', ( #6766, #11239, #12035, #5070 ) ) ;
#3091 = CARTESIAN_POINT ( 'NONE',  ( -80.90000000000000568, -30.75000000000000355, -97.40192378864668399 ) ) ;
#3092 = CARTESIAN_POINT ( 'NONE',  ( 4.055487192203242941, 1.409979666030558354, -3.568038521265956664 ) ) ;
#3093 = CARTESIAN_POINT ( 'NONE',  ( -83.90000000000000568, -34.96874999877096712, -102.5980762113533018 ) ) ;
#3094 = B_SPLINE_CURVE_WITH_KNOTS ( 'NONE', 3,
 ( #12030, #13494, #3042, #18001, #5890, #7443 ),
 .UNSPECIFIED., .F., .F.,
 ( 4, 2, 4 ),
 ( 0.002365888236227995517, 0.003551327329835084114, 0.004736766423442172712 ),
 .UNSPECIFIED. ) ;
#3095 = CARTESIAN_POINT ( 'NONE',  ( -85.15643035624999868, -33.89062499938548711, -101.5914258081833879 ) ) ;
#3096 = CARTESIAN_POINT ( 'NONE',  ( 231.7961524227065979, -33.63615380933863008, -53.00000000000011369 ) ) ;
#3097 = CARTESIAN_POINT ( 'NONE',  ( 232.5999999999999375, -30.81562499938547717, 96.81714838363319586 ) ) ;
#3098 = CARTESIAN_POINT ( 'NONE',  ( -80.90000000000000568, -32.94768749875867542, 102.5980762113533018 ) ) ;
#3099 = EDGE_CURVE ( 'NONE', #1391, #3532, #10613, .T. ) ;
#3100 = CARTESIAN_POINT ( 'NONE',  ( -85.15643035624999868, -34.79062499938548569, 98.40857419181659793 ) ) ;
#3101 = CARTESIAN_POINT ( 'NONE',  ( 235.5999999999999943, -33.80624999877096570, 101.7320508075688537 ) ) ;
#3102 = MANIFOLD_SOLID_BREP ( 'Cavity1', #6354 ) ;
#3103 = CARTESIAN_POINT ( 'NONE',  ( 81.02178482187500208, -34.04062499938548569, 97.61286128772489690 ) ) ;
#3104 = FACE_OUTER_BOUND ( 'NONE', #2055, .T. ) ;
#3105 = CARTESIAN_POINT ( 'NONE',  ( -82.40000000000000568, -30.00000000000000355, 103.0000000000000000 ) ) ;
#3106 = CARTESIAN_POINT ( 'NONE',  ( 79.39999999999999147, -33.80624999877097281, -101.7320508075688537 ) ) ;
#3107 = CARTESIAN_POINT ( 'NONE',  ( 234.0999999999999375, -33.44999999999999574, 102.5980762113533018 ) ) ;
#3108 = ORIENTED_EDGE ( 'NONE', *, *, #19189, .F. ) ;
#3109 = CARTESIAN_POINT ( 'NONE',  ( 235.3564303562499447, -32.72812499938547859, -50.00000000000011369 ) ) ;
#3110 = CARTESIAN_POINT ( 'NONE',  ( 235.3564303562499447, -30.51562499938548001, 101.5914258081833879 ) ) ;
#3111 = CARTESIAN_POINT ( 'NONE',  ( 235.5999999999999943, -32.83124999877095718, -51.73205080756900287 ) ) ;
#3112 = CARTESIAN_POINT ( 'NONE',  ( -79.64356964374999848, -32.61562499938548854, 99.99999999999998579 ) ) ;
#3113 = ORIENTED_EDGE ( 'NONE', *, *, #4119, .F. ) ;
#3114 = ORIENTED_EDGE ( 'NONE', *, *, #18600, .F. ) ;
#3115 = CARTESIAN_POINT ( 'NONE',  ( -81.22643902601926413, -32.00000000000000000, 97.33634050170186924 ) ) ;
#3116 = CARTESIAN_POINT ( 'NONE',  ( 231.0999999999999375, -34.87499999999999289, 102.5980762113533018 ) ) ;
#3117 = DIRECTION ( 'NONE',  ( 0.000000000000000000, -0.8660254037844382635, -0.5000000000000008882 ) ) ;
#3118 = ORIENTED_EDGE ( 'NONE', *, *, #5910, .T. ) ;
#3119 = CARTESIAN_POINT ( 'NONE',  ( -82.40000000000000568, -50.00000000000000000, 92.49999999999997158 ) ) ;
#3120 = CARTESIAN_POINT ( 'NONE',  ( 232.5999999999999375, -33.88124999877096855, 102.9999999999999858 ) ) ;
#3121 =( BOUNDED_CURVE ( )  B_SPLINE_CURVE ( 2, ( #4705, #5976, #15247, #6362, #321, #3127, #126, #9086, #6076 ),
 .UNSPECIFIED., .F., .F. ) 
 B_SPLINE_CURVE_WITH_KNOTS ( ( 3, 2, 2, 2, 3 ),
 ( 0.6041666666666666297, 0.6111111111111111605, 0.6250000000000000000, 0.6388888888888888395, 0.6458333333333332593 ),
 .UNSPECIFIED. ) 
 CURVE ( )  GEOMETRIC_REPRESENTATION_ITEM ( )  RATIONAL_B_SPLINE_CURVE ( ( 0.9330127018922192983, 0.9330127018922187432, 1.000000000000000000, 0.8660254037844387076, 1.000000000000000000, 0.8660254037844387076, 1.000000000000000000, 0.9330127018922198534, 0.9330127018922192983 ) ) 
 REPRESENTATION_ITEM ( '' )  );
#3122 = CARTESIAN_POINT ( 'NONE',  ( -79.64356964375001269, -33.66562499938549280, 101.5914258081833879 ) ) ;
#3123 = CARTESIAN_POINT ( 'NONE',  ( -80.90000000000000568, -30.54374999877096997, 97.40192378864668399 ) ) ;
#3124 = CARTESIAN_POINT ( 'NONE',  ( -85.40000000000000568, -30.84374999877096712, 99.99999999999998579 ) ) ;
#3125 = CARTESIAN_POINT ( 'NONE',  ( 232.5999999999999375, -33.48749999999999716, 103.0000000000000000 ) ) ;
#3126 = DIRECTION ( 'NONE',  ( 0.000000000000000000, -1.000000000000000000, 0.000000000000000000 ) ) ;
#3127 = CARTESIAN_POINT ( 'NONE',  ( -79.39999999999999147, -33.41250000000000142, 101.7320508075688537 ) ) ;
#3128 = CARTESIAN_POINT ( 'NONE',  ( -79.64057174634722003, -35.00000000000000000, -99.60353574117785058 ) ) ;
#3129 = CARTESIAN_POINT ( 'NONE',  ( 235.3564303562499447, -31.71562499938547575, 99.99999999999998579 ) ) ;
#3130 = VERTEX_POINT ( 'NONE', #15012 ) ;
#3131 = SURFACE_STYLE_USAGE ( .BOTH. , #18189 ) ;
#3132 = CARTESIAN_POINT ( 'NONE',  ( -82.39999999999999147, -34.30312499938548143, -103.1828516163667899 ) ) ;
#3133 = CARTESIAN_POINT ( 'NONE',  ( 234.0999999999999375, -33.39374999877096428, -47.40192378864679768 ) ) ;
#3134 = CARTESIAN_POINT ( 'NONE',  ( 244.7999999999999545, -4.999999999999990230, -100.0000000000000995 ) ) ;
#3135 = LINE ( 'NONE', #11935, #9599 ) ;
#3136 = CARTESIAN_POINT ( 'NONE',  ( -79.64356964375001269, -33.47812499938547859, 98.40857419181659793 ) ) ;
#3137 = DIRECTION ( 'NONE',  ( 0.000000000000000000, 0.000000000000000000, -1.000000000000000000 ) ) ;
#3138 = CARTESIAN_POINT ( 'NONE',  ( 229.8435696437499303, -35.09062499938547575, -50.00000000000011369 ) ) ;
#3139 = EDGE_LOOP ( 'NONE', ( #16917, #3061, #16609, #1684 ) ) ;
#3140 = ORIENTED_EDGE ( 'NONE', *, *, #6608, .T. ) ;
#3141 = PLANE ( 'NONE',  #15070 ) ;
#3142 = CARTESIAN_POINT ( 'NONE',  ( -83.90000000000000568, -30.52500000000000213, 97.40192378864668399 ) ) ;
#3143 = EDGE_CURVE ( 'NONE', #8999, #13758, #9728, .T. ) ;
#3144 = CARTESIAN_POINT ( 'NONE',  ( -80.90000000000000568, -32.94374999877096855, 102.5980762113533018 ) ) ;
#3145 = CARTESIAN_POINT ( 'NONE',  ( 79.39999999999999147, -31.53750000000000497, 101.7320508075688821 ) ) ;
#3146 = DIRECTION ( 'NONE',  ( 1.000000000000000000, 0.000000000000000000, -0.000000000000000000 ) ) ;
#3147 = CARTESIAN_POINT ( 'NONE',  ( 232.5999999999999375, -34.75312499938547717, 96.81714838363319586 ) ) ;
#3148 = CARTESIAN_POINT ( 'NONE',  ( 235.3564303562499447, -34.86562499938547433, -50.00000000000011369 ) ) ;
#3149 = CARTESIAN_POINT ( 'NONE',  ( 80.90000000000000568, -33.45000000000000284, -102.5980762113533018 ) ) ;
#3150 = CARTESIAN_POINT ( 'NONE',  ( 85.15643035624999868, -32.35312499938549280, -101.5914258081833879 ) ) ;
#3151 = ORIENTED_EDGE ( 'NONE', *, *, #11313, .F. ) ;
#3153 = EDGE_CURVE ( 'NONE', #7460, #6753, #5346, .T. ) ;
#3152 = CARTESIAN_POINT ( 'NONE',  ( 229.5999999999999375, -32.66249999999999432, -48.26794919243123161 ) ) ;
#3154 = DIRECTION ( 'NONE',  ( 5.139921410301648824E-16, 1.000000000000000000, -3.597944987211154374E-15 ) ) ;
#3155 = CARTESIAN_POINT ( 'NONE',  ( 83.77821517812500929, -32.31562499938548427, -102.3871387122750889 ) ) ;
#3156 = ADVANCED_FACE ( 'NONE', ( #18725 ), #3279, .F. ) ;
#3157 = FACE_OUTER_BOUND ( 'NONE', #15930, .T. ) ;
#3158 = CARTESIAN_POINT ( 'NONE',  ( -79.39999999999999147, -34.63124999877096855, 98.26794919243110371 ) ) ;
#3159 = CARTESIAN_POINT ( 'NONE',  ( 229.8435696437499871, -30.29062499938548214, -51.59142580818350865 ) ) ;
#3160 = ADVANCED_FACE ( 'NONE', ( #10873 ), #18215, .T. ) ;
#3161 = CARTESIAN_POINT ( 'NONE',  ( -83.77821517812500929, -34.71562499938548285, 97.61286128772489690 ) ) ;
#3162 = ORIENTED_EDGE ( 'NONE', *, *, #7927, .T. ) ;
#3163 = CARTESIAN_POINT ( 'NONE',  ( -83.18600968418431307, -35.00069049296057955, 102.9003918199492915 ) ) ;
#3164 = MANIFOLD_SOLID_BREP ( 'M5 Clearance Hole1', #13153 ) ;
#3165 = CARTESIAN_POINT ( 'NONE',  ( 229.8435696437499303, -34.19062499938547717, 99.99999999999998579 ) ) ;
#3166 = CARTESIAN_POINT ( 'NONE',  ( -94.79999999999999716, -3.000000000000000000, -150.0000000000000000 ) ) ;
#3167 =( BOUNDED_CURVE ( )  B_SPLINE_CURVE ( 2, ( #15636, #16999, #2241, #4999, #17196, #3516, #9571, #9769, #3900 ),
 .UNSPECIFIED., .F., .F. ) 
 B_SPLINE_CURVE_WITH_KNOTS ( ( 3, 2, 2, 2, 3 ),
 ( 0.6875000000000000000, 0.6944444444444444198, 0.7083333333333333703, 0.7222222222222222099, 0.7291666666666666297 ),
 .UNSPECIFIED. ) 
 CURVE ( )  GEOMETRIC_REPRESENTATION_ITEM ( )  RATIONAL_B_SPLINE_CURVE ( ( 0.9330127018922194093, 0.9330127018922194093, 1.000000000000000000, 0.8660254037844387076, 1.000000000000000000, 0.8660254037844387076, 1.000000000000000000, 0.9330127018922198534, 0.9330127018922192983 ) ) 
 REPRESENTATION_ITEM ( '' )  );
#3168 = CARTESIAN_POINT ( 'NONE',  ( -82.39999999999999147, -31.90856250001229810, 96.53589838486223584 ) ) ;
#3169 = CARTESIAN_POINT ( 'NONE',  ( 94.79999999999984084, 0.000000000000000000, -150.0000000000000000 ) ) ;
#3170 = EDGE_CURVE ( 'NONE', #1228, #7532, #8516, .T. ) ;
#3171 = CARTESIAN_POINT ( 'NONE',  ( -82.39999999999999147, -32.36250000000000426, 96.99999999999997158 ) ) ;
#3172 = CARTESIAN_POINT ( 'NONE',  ( 82.39999999999999147, -30.70312499938548711, 103.1828516163667899 ) ) ;
#3173 = LINE ( 'NONE', #265, #18340 ) ;
#3174 = CARTESIAN_POINT ( 'NONE',  ( 232.5999999999999375, -31.37812499938547717, -46.81714838363331666 ) ) ;
#3175 = FACE_OUTER_BOUND ( 'NONE', #9076, .T. ) ;
#3176 = CARTESIAN_POINT ( 'NONE',  ( -85.15643035624999868, -32.09062499938548996, -101.5914258081833879 ) ) ;
#3177 = ORIENTED_EDGE ( 'NONE', *, *, #18192, .T. ) ;
#3178 = CARTESIAN_POINT ( 'NONE',  ( 82.39999999999999147, -31.49062499938548854, 96.81714838363319586 ) ) ;
#3179 = DIRECTION ( 'NONE',  ( 0.000000000000000000, 0.000000000000000000, -1.000000000000000000 ) ) ;
#3180 = AXIS2_PLACEMENT_3D ( 'NONE', #15910, #8669, #8472 ) ;
#3181 = CARTESIAN_POINT ( 'NONE',  ( -83.20384757729335945, -33.05759618943233136, 102.9999999999999858 ) ) ;
#3182 = MECHANICAL_DESIGN_GEOMETRIC_PRESENTATION_REPRESENTATION (  '', ( #3490 ), #12228 ) ;
#3183 = CARTESIAN_POINT ( 'NONE',  ( -85.15643035625001289, -31.60312499938548569, 99.99999999999998579 ) ) ;
#3184 = CARTESIAN_POINT ( 'NONE',  ( 83.20384757729333103, -33.18615380933863435, 103.0000000000000000 ) ) ;
#3185 = VERTEX_POINT ( 'NONE', #9405 ) ;
#3186 = EDGE_CURVE ( 'NONE', #12568, #1155, #11648, .T. ) ;
#3187 = CARTESIAN_POINT ( 'NONE',  ( -83.90000000000000568, -32.32500000000000284, -102.5980762113533018 ) ) ;
#3188 = CARTESIAN_POINT ( 'NONE',  ( 4.050823680195225762, -2.400527758044907589, -2.978030508226147788 ) ) ;
#3189 = CARTESIAN_POINT ( 'NONE',  ( -85.40000000000000568, -34.89374999877097139, -99.99999999999998579 ) ) ;
#3190 = CARTESIAN_POINT ( 'NONE',  ( -82.39999999999999147, -33.29062499938549280, -96.81714838363319586 ) ) ;
#3191 = DIRECTION ( 'NONE',  ( 2.407412430484046130E-31, -3.340955887615246502E-46, 1.000000000000000000 ) ) ;
#3192 = CARTESIAN_POINT ( 'NONE',  ( 235.3564303562499447, -33.62812499938547717, 99.99999999999998579 ) ) ;
#3193 = CARTESIAN_POINT ( 'NONE',  ( -79.39999999999999147, -30.66018749875867755, 101.7320508075688537 ) ) ;
#3194 = ORIENTED_EDGE ( 'NONE', *, *, #18015, .F. ) ;
#3195 = CARTESIAN_POINT ( 'NONE',  ( -85.15643035624999868, -33.89062499938548711, 98.40857419181659793 ) ) ;
#3196 = CARTESIAN_POINT ( 'NONE',  ( 232.5999999999999375, -33.88124999877096855, 102.9999999999999858 ) ) ;
#3197 = CARTESIAN_POINT ( 'NONE',  ( 83.77821517812500929, -32.91562499938547859, 102.3871387122750889 ) ) ;
#3198 = CARTESIAN_POINT ( 'NONE',  ( 105.1999999999999886, -29.79999999999997229, -103.0000000000000142 ) ) ;
#3199 = VECTOR ( 'NONE', #12599, 1000.000000000000000 ) ;
#3200 = LINE ( 'NONE', #7506, #12695 ) ;
#3201 = CARTESIAN_POINT ( 'NONE',  ( 85.40000000000000568, -33.58124999877097139, -98.26794919243111792 ) ) ;
#3202 = CARTESIAN_POINT ( 'NONE',  ( 235.5999999999999375, -32.47499999999999432, 99.99999999999998579 ) ) ;
#3203 = ORIENTED_EDGE ( 'NONE', *, *, #5324, .T. ) ;
#3204 = CARTESIAN_POINT ( 'NONE',  ( 231.2217848218749339, -33.47812499938547859, -52.38713871227520968 ) ) ;
#3205 = DIRECTION ( 'NONE',  ( 0.000000000000000000, 0.000000000000000000, -1.000000000000000000 ) ) ;
#3206 = CARTESIAN_POINT ( 'NONE',  ( 235.3564303562499447, -30.89062499938548001, 98.40857419181659793 ) ) ;
#3207 = CARTESIAN_POINT ( 'NONE',  ( 232.5999999999999375, -35.00624999877096855, -53.46410161513786363 ) ) ;
#3208 =( REPRESENTATION_RELATIONSHIP ('NONE','NONE', #14468, #16991 ) REPRESENTATION_RELATIONSHIP_WITH_TRANSFORMATION ( #2414 )SHAPE_REPRESENTATION_RELATIONSHIP( ) );
#3209 = CARTESIAN_POINT ( 'NONE',  ( -79.64356964374998427, -34.00312499938548427, 101.5914258081833879 ) ) ;
#3210 = ORIENTED_EDGE ( 'NONE', *, *, #13066, .T. ) ;
#3211 = VERTEX_POINT ( 'NONE', #14284 ) ;
#3212 = CARTESIAN_POINT ( 'NONE',  ( 229.5999999999999375, -32.60624999877096286, -48.26794919243123161 ) ) ;
#3213 = AXIS2_PLACEMENT_3D ( 'NONE', #8648, #15988, #18834 ) ;
#3214 = FACE_BOUND ( 'NONE', #6954, .T. ) ;
#3215 = CARTESIAN_POINT ( 'NONE',  ( -79.39999999999999147, -34.72500000000000142, 99.99999999999998579 ) ) ;
#3216 = ORIENTED_EDGE ( 'NONE', *, *, #2563, .T. ) ;
#3217 = CARTESIAN_POINT ( 'NONE',  ( -83.90000000000000568, -31.36874999877096926, 97.40192378864668399 ) ) ;
#3218 = CARTESIAN_POINT ( 'NONE',  ( 99.99999999999998579, -1.387778780781445676E-13, -2.407412430484045937E-29 ) ) ;
#3219 = CARTESIAN_POINT ( 'NONE',  ( -82.39999999999999147, -33.74062499938548854, 103.1828516163667899 ) ) ;
#3220 = CARTESIAN_POINT ( 'NONE',  ( -82.39999999999999147, -34.16250000000000142, 96.53589838486223584 ) ) ;
#3221 = CARTESIAN_POINT ( 'NONE',  ( -85.40000000000000568, -31.25624999877096855, 101.7320508075688679 ) ) ;
#3222 = FACE_OUTER_BOUND ( 'NONE', #204, .T. ) ;
#3223 = DIRECTION ( 'NONE',  ( -1.000000000000000000, 1.387778780781445676E-15, 2.407412430484046130E-31 ) ) ;
#3224 = DIRECTION ( 'NONE',  ( -0.000000000000000000, -0.000000000000000000, 1.000000000000000000 ) ) ;
#3225 = CARTESIAN_POINT ( 'NONE',  ( 105.1999999999999744, -29.80000000000000071, 150.0000000000000000 ) ) ;
#3226 = CARTESIAN_POINT ( 'NONE',  ( 235.3564303562499447, -31.67812499938547788, 98.40857419181659793 ) ) ;
#3227 = EDGE_LOOP ( 'NONE', ( #15134, #19037 ) ) ;
#3228 =( NAMED_UNIT ( * ) SI_UNIT ( $, .STERADIAN. ) SOLID_ANGLE_UNIT ( ) );
#3229 = CARTESIAN_POINT ( 'NONE',  ( -79.64356964374999848, -32.16562499938548569, -99.99999999999998579 ) ) ;
#3230 = CARTESIAN_POINT ( 'NONE',  ( 4.132952817037860882, 4.063368025374524350, -1.550749365883601148E-16 ) ) ;
#3231 = CARTESIAN_POINT ( 'NONE',  ( -85.40000000000000568, -32.64374999877097139, 99.99999999999998579 ) ) ;
#3232 = CARTESIAN_POINT ( 'NONE',  ( 230.4006479041978821, -35.00000000000000711, -48.20719995774843625 ) ) ;
#3233 = DIRECTION ( 'NONE',  ( -1.000000000000000000, 0.000000000000000000, 0.000000000000000000 ) ) ;
#3234 =( BOUNDED_CURVE ( )  B_SPLINE_CURVE ( 2, ( #1623, #1340, #15005, #6118, #4362, #13623, #10322, #19214, #19318 ),
 .UNSPECIFIED., .F., .F. ) 
 B_SPLINE_CURVE_WITH_KNOTS ( ( 3, 2, 2, 2, 3 ),
 ( 0.4791666666666666297, 0.4861111111111111049, 0.5000000000000000000, 0.5138888888888888395, 0.5208333333333333703 ),
 .UNSPECIFIED. ) 
 CURVE ( )  GEOMETRIC_REPRESENTATION_ITEM ( )  RATIONAL_B_SPLINE_CURVE ( ( 0.9330127018922194093, 0.9330127018922190762, 1.000000000000000000, 0.8660254037844387076, 1.000000000000000000, 0.8660254037844387076, 1.000000000000000000, 0.9330127018922187432, 0.9330127018922192983 ) ) 
 REPRESENTATION_ITEM ( '' )  );
#3235 = ORIENTED_EDGE ( 'NONE', *, *, #13289, .F. ) ;
#3236 = ORIENTED_EDGE ( 'NONE', *, *, #4702, .T. ) ;
#3237 = B_SPLINE_CURVE_WITH_KNOTS ( 'NONE', 3,
 ( #16713, #18096, #4706, #13681, #15051, #3320 ),
 .UNSPECIFIED., .F., .F.,
 ( 4, 2, 4 ),
 ( 0.003358874760055551890, 0.004541967308452098118, 0.005725059856848645212 ),
 .UNSPECIFIED. ) ;
#3238 = CARTESIAN_POINT ( 'NONE',  ( 79.39999999999999147, -33.28124999877096712, -98.26794919243110371 ) ) ;
#3239 = CARTESIAN_POINT ( 'NONE',  ( -85.40000000000000568, -31.83750000000000568, 98.26794919243111792 ) ) ;
#3240 = CARTESIAN_POINT ( 'NONE',  ( -82.39999999999999147, -32.98124999877096997, 103.4641016151377499 ) ) ;
#3241 = CARTESIAN_POINT ( 'NONE',  ( 85.40000000000000568, -30.86250000000000071, 98.26794919243111792 ) ) ;
#3242 = CARTESIAN_POINT ( 'NONE',  ( -69.99999999999998579, -32.00000000000000000, -150.0000000000000000 ) ) ;
#3243 = CARTESIAN_POINT ( 'NONE',  ( 232.5999999999999375, -34.52812499938548285, 103.1828516163667899 ) ) ;
#3244 = CARTESIAN_POINT ( 'NONE',  ( 81.22643902596138332, -31.99999999999999289, -97.33634050172426555 ) ) ;
#3245 = EDGE_CURVE ( 'NONE', #15781, #10258, #9799, .T. ) ;
#3246 = CARTESIAN_POINT ( 'NONE',  ( 82.39999999999999147, -34.52812499938548996, -103.1828516163667899 ) ) ;
#3247 = ORIENTED_EDGE ( 'NONE', *, *, #17486, .T. ) ;
#3248 = CARTESIAN_POINT ( 'NONE',  ( 229.5999999999999375, -33.56249999999999289, -48.26794919243123161 ) ) ;
#3249 = CARTESIAN_POINT ( 'NONE',  ( -85.40000000000000568, -34.01250000000000284, 101.7320508075688821 ) ) ;
#3250 = CARTESIAN_POINT ( 'NONE',  ( 81.02178482187500208, -34.04062499938548569, -102.3871387122750889 ) ) ;
#3251 = EDGE_CURVE ( 'NONE', #3695, #11212, #1200, .T. ) ;
#3252 = ADVANCED_FACE ( 'NONE', ( #18889 ), #10179, .F. ) ;
#3253 = DIRECTION ( 'NONE',  ( -0.000000000000000000, 3.469446951953616161E-16, -1.000000000000000000 ) ) ;
#3254 = CARTESIAN_POINT ( 'NONE',  ( -85.15643035624999868, -32.09062499938548996, 98.40857419181659793 ) ) ;
#3255 = CARTESIAN_POINT ( 'NONE',  ( 229.8435696437499871, -33.89062499938548001, -51.59142580818350865 ) ) ;
#3256 = CARTESIAN_POINT ( 'NONE',  ( -85.15643035624999868, -35.05312499938548143, 101.5914258081833879 ) ) ;
#3257 = ORIENTED_EDGE ( 'NONE', *, *, #14718, .F. ) ;
#3258 = CARTESIAN_POINT ( 'NONE',  ( -79.43507259642450435, -35.00111651776678201, 99.51279508880003277 ) ) ;
#3259 = CARTESIAN_POINT ( 'NONE',  ( 233.9782151781249411, -34.79062499938547859, 97.61286128772489690 ) ) ;
#3260 = CARTESIAN_POINT ( 'NONE',  ( -80.90000000000000568, -32.55000000000000426, 102.5980762113533018 ) ) ;
#3261 = CARTESIAN_POINT ( 'NONE',  ( -82.39999999999999147, -34.38356250001228176, 103.4641016151377499 ) ) ;
#3262 = EDGE_CURVE ( 'NONE', #5496, #1022, #7739, .T. ) ;
#3263 = CARTESIAN_POINT ( 'NONE',  ( 234.0999999999999375, -34.64999999999999147, 97.40192378864668399 ) ) ;
#3264 = EDGE_CURVE ( 'NONE', #12007, #12136, #13344, .T. ) ;
#3265 = CARTESIAN_POINT ( 'NONE',  ( -79.64356964374998427, -31.86562499938548143, 101.5914258081833879 ) ) ;
#3266 = CARTESIAN_POINT ( 'NONE',  ( 84.82992844608111227, -32.00000000000000000, 101.3134070403133080 ) ) ;
#3267 = CARTESIAN_POINT ( 'NONE',  ( 85.15643035625001289, -35.20312499938548711, 99.99999999999998579 ) ) ;
#3268 = EDGE_CURVE ( 'NONE', #11655, #14259, #4127, .T. ) ;
#3269 = CARTESIAN_POINT ( 'NONE',  ( 85.15643035625001289, -32.05312499938548854, -99.99999999999998579 ) ) ;
#3270 = CARTESIAN_POINT ( 'NONE',  ( 231.2217848218749339, -30.51562499938548001, -47.61286128772501769 ) ) ;
#3271 = CARTESIAN_POINT ( 'NONE',  ( -85.12124608221316180, -32.00000000000002132, -100.4735569575799445 ) ) ;
#3272 = CARTESIAN_POINT ( 'NONE',  ( -83.77821517812500929, -33.47812499938548569, -102.3871387122750889 ) ) ;
#3273 = ORIENTED_EDGE ( 'NONE', *, *, #12900, .T. ) ;
#3274 = CARTESIAN_POINT ( 'NONE',  ( 79.39999999999999147, -34.66874999877096997, 99.99999999999998579 ) ) ;
#3275 = DIRECTION ( 'NONE',  ( 0.000000000000000000, 0.000000000000000000, 1.000000000000000000 ) ) ;
#3276 = AXIS2_PLACEMENT_3D ( 'NONE', #13544, #12281, #6041 ) ;
#3277 = DIRECTION ( 'NONE',  ( 0.000000000000000000, 0.000000000000000000, 1.000000000000000000 ) ) ;
#3278 = CARTESIAN_POINT ( 'NONE',  ( -81.02178482187500208, -31.90312499938548996, 102.3871387122750889 ) ) ;
#3279 =( BOUNDED_SURFACE ( )  B_SPLINE_SURFACE ( 1, 2, ( 
 ( #3570, #12756, #14310, #3861, #9430, #13921, #658, #2007, #14023, #2296, #15495, #18428, #6706, #14210, #5048, #5243, #11286, #17255, #6606, #6810, #8165, #847, #10897, #948, #9823, #3763, #15397, #7967, #11088, #3670, #12653, #3471, #2394, #10992, #16959, #751, #9530, #17155, #6903, #2108, #18625, #8356, #8069, #12851, #12555, #4956, #9635, #17057, #11192, #15596, #16865, #2204, #14114, #17541, #8449, #14792, #16175, #4159, #10309, #2785, #5632, #8737, #5725, #16267, #15886, #8638, #8836, #13229, #19102, #14595, #18916, #2878, #5819, #18823, #14691, #1325, #11767, #7182, #1419, #3959, #9925, #5535, #7372, #16072, #5445, #10117, #2491, #12944, #11578, #14401, #2681, #1040, #7275, #14495, #19203, #6993, #1227, #13131, #17743, #11483, #4349, #11383, #17349, #11674, #17449, #4060, #10020, #15979, #2583, #17638, #8544, #1128, #7085, #13041, #19012, #4253, #10212, #4537, #1520, #355, #14992, #10595, #3161, #6209, #4740, #9314, #7654, #4645, #2972, #15178, #1795, #3256, #9121, #10400, #10686, #9030, #7471 ),
 ( #4442, #58, #15085, #16362, #12157, #15278, #13428, #1702, #4838, #10497, #7759, #8928, #13328, #18221, #6302, #16653, #9212, #18125, #13610, #16559, #252, #11958, #7563, #17928, #13714, #12252, #13519, #16744, #10781, #156, #6107, #14890, #3357, #1893, #19304, #3068, #5917, #11863, #17830, #6007, #16461, #1614, #12056, #18032, #6396, #12443, #5031, #15476, #448, #12536, #12349, #3453, #2089, #18315, #14002, #14096, #9410, #8044, #2188, #1992, #5126, #4934, #7851, #8144, #15575, #11069, #17039, #6589, #640, #9510, #18508, #15375, #18411, #7948, #9614, #3650, #10971, #735, #6689, #16941, #3553, #13806, #10878, #16849, #13901, #538, #6494, #3621, #17033, #2081, #1985, #15664, #3643, #18406, #11164, #9605, #6486, #15570, #6584, #17131, #16739, #9503, #9702, #14091, #634, #15471, #443, #3737, #6684, #351, #2181, #8139, #12627, #8038, #2274, #4834, #10775, #6389, #8238, #16937, #6297, #10967, #3349, #13800, #12438, #9309, #3548, #15272, #731, #15370, #18601, #1887, #5026, #13994, #5216, #7846, #12248 ) ),
 .UNSPECIFIED., .F., .F., .F. ) 
 B_SPLINE_SURFACE_WITH_KNOTS ( ( 2, 2 ),
 ( 3, 2, 2, 2, 2, 2, 2, 2, 2, 2, 2, 2, 2, 2, 2, 2, 2, 2, 2, 2, 2, 2, 2, 2, 2, 2, 2, 2, 2, 2, 2, 2, 2, 2, 2, 2, 2, 2, 2, 2, 2, 2, 2, 2, 2, 2, 2, 2, 2, 2, 2, 2, 2, 2, 2, 2, 2, 2, 2, 2, 2, 2, 2, 2, 2, 2, 2, 2, 3 ),
 ( 0.000000000000000000, 1.000000000000000000 ),
 ( 0.000000000000000000, 0.01388888888888888812, 0.02777777777777777624, 0.04166666666666666435, 0.05555555555555555247, 0.06944444444444444753, 0.08333333333333332871, 0.09722222222222222376, 0.1111111111111111049, 0.1250000000000000000, 0.1388888888888888951, 0.1527777777777777901, 0.1666666666666666574, 0.1805555555555555525, 0.1944444444444444475, 0.2083333333333333426, 0.2222222222222222099, 0.2361111111111111049, 0.2500000000000000000, 0.2638888888888888951, 0.2777777777777777901, 0.2916666666666666852, 0.3055555555555555802, 0.3194444444444444198, 0.3333333333333333148, 0.3472222222222222099, 0.3611111111111111049, 0.3750000000000000000, 0.3888888888888888951, 0.4027777777777777901, 0.4166666666666666852, 0.4305555555555555802, 0.4444444444444444198, 0.4583333333333333148, 0.4722222222222222099, 0.4861111111111111049, 0.5000000000000000000, 0.5138888888888888395, 0.5277777777777777901, 0.5416666666666666297, 0.5555555555555555802, 0.5694444444444444198, 0.5833333333333333703, 0.5972222222222222099, 0.6111111111111111605, 0.6250000000000000000, 0.6388888888888888395, 0.6527777777777777901, 0.6666666666666666297, 0.6805555555555555802, 0.6944444444444444198, 0.7083333333333333703, 0.7222222222222222099, 0.7361111111111111605, 0.7500000000000000000, 0.7638888888888888395, 0.7777777777777777901, 0.7916666666666666297, 0.8055555555555555802, 0.8194444444444444198, 0.8333333333333333703, 0.8472222222222222099, 0.8611111111111111605, 0.8750000000000000000, 0.8888888888888888395, 0.9027777777777777901, 0.9166666666666666297, 0.9258785066912882389, 0.9351372917582011501 ),
 .UNSPECIFIED. ) 
 GEOMETRIC_REPRESENTATION_ITEM ( )  RATIONAL_B_SPLINE_SURFACE ( (
 ( 1.000000000000000000, 0.8660254037844387076, 1.000000000000000000, 0.8660254037844387076, 1.000000000000000000, 0.8660254037844387076, 1.000000000000000000, 0.8660254037844387076, 1.000000000000000000, 0.8660254037844387076, 1.000000000000000000, 0.8660254037844387076, 1.000000000000000000, 0.8660254037844387076, 1.000000000000000000, 0.8660254037844387076, 1.000000000000000000, 0.8660254037844387076, 1.000000000000000000, 0.8660254037844387076, 1.000000000000000000, 0.8660254037844387076, 1.000000000000000000, 0.8660254037844387076, 1.000000000000000000, 0.8660254037844387076, 1.000000000000000000, 0.8660254037844387076, 1.000000000000000000, 0.8660254037844387076, 1.000000000000000000, 0.8660254037844387076, 1.000000000000000000, 0.8660254037844387076, 1.000000000000000000, 0.8660254037844387076, 1.000000000000000000, 0.8660254037844387076, 1.000000000000000000, 0.8660254037844387076, 1.000000000000000000, 0.8660254037844387076, 1.000000000000000000, 0.8660254037844387076, 1.000000000000000000, 0.8660254037844387076, 1.000000000000000000, 0.8660254037844387076, 1.000000000000000000, 0.8660254037844387076, 1.000000000000000000, 0.8660254037844387076, 1.000000000000000000, 0.8660254037844387076, 1.000000000000000000, 0.8660254037844387076, 1.000000000000000000, 0.8660254037844387076, 1.000000000000000000, 0.8660254037844387076, 1.000000000000000000, 0.8660254037844387076, 1.000000000000000000, 0.8660254037844387076, 1.000000000000000000, 0.8660254037844387076, 1.000000000000000000, 0.8660254037844387076, 1.000000000000000000, 0.8660254037844387076, 1.000000000000000000, 0.8660254037844387076, 1.000000000000000000, 0.8660254037844387076, 1.000000000000000000, 0.8660254037844387076, 1.000000000000000000, 0.8660254037844387076, 1.000000000000000000, 0.8660254037844387076, 1.000000000000000000, 0.8660254037844387076, 1.000000000000000000, 0.8660254037844387076, 1.000000000000000000, 0.8660254037844387076, 1.000000000000000000, 0.8660254037844387076, 1.000000000000000000, 0.8660254037844387076, 1.000000000000000000, 0.8660254037844387076, 1.000000000000000000, 0.8660254037844387076, 1.000000000000000000, 0.8660254037844387076, 1.000000000000000000, 0.8660254037844387076, 1.000000000000000000, 0.8660254037844387076, 1.000000000000000000, 0.8660254037844387076, 1.000000000000000000, 0.8660254037844387076, 1.000000000000000000, 0.8660254037844387076, 1.000000000000000000, 0.8660254037844387076, 1.000000000000000000, 0.8660254037844387076, 1.000000000000000000, 0.8660254037844387076, 1.000000000000000000, 0.8660254037844387076, 1.000000000000000000, 0.8660254037844387076, 1.000000000000000000, 0.8660254037844387076, 1.000000000000000000, 0.8660254037844387076, 1.000000000000000000, 0.8660254037844387076, 1.000000000000000000, 0.8660254037844387076, 1.000000000000000000, 0.8660254037844387076, 1.000000000000000000, 0.8660254037844387076, 1.000000000000000000, 0.8660254037844387076, 1.000000000000000000, 0.8660254037844387076, 1.000000000000000000, 0.9111410165655264848, 0.9401539157124900736, 0.9401539157124900736, 0.9401539157124900736),
 ( 1.000000000000000000, 0.8660254037844387076, 1.000000000000000000, 0.8660254037844387076, 1.000000000000000000, 0.8660254037844387076, 1.000000000000000000, 0.8660254037844387076, 1.000000000000000000, 0.8660254037844387076, 1.000000000000000000, 0.8660254037844387076, 1.000000000000000000, 0.8660254037844387076, 1.000000000000000000, 0.8660254037844387076, 1.000000000000000000, 0.8660254037844387076, 1.000000000000000000, 0.8660254037844387076, 1.000000000000000000, 0.8660254037844387076, 1.000000000000000000, 0.8660254037844387076, 1.000000000000000000, 0.8660254037844387076, 1.000000000000000000, 0.8660254037844387076, 1.000000000000000000, 0.8660254037844387076, 1.000000000000000000, 0.8660254037844387076, 1.000000000000000000, 0.8660254037844387076, 1.000000000000000000, 0.8660254037844387076, 1.000000000000000000, 0.8660254037844387076, 1.000000000000000000, 0.8660254037844387076, 1.000000000000000000, 0.8660254037844387076, 1.000000000000000000, 0.8660254037844387076, 1.000000000000000000, 0.8660254037844387076, 1.000000000000000000, 0.8660254037844387076, 1.000000000000000000, 0.8660254037844387076, 1.000000000000000000, 0.8660254037844387076, 1.000000000000000000, 0.8660254037844387076, 1.000000000000000000, 0.8660254037844387076, 1.000000000000000000, 0.8660254037844387076, 1.000000000000000000, 0.8660254037844387076, 1.000000000000000000, 0.8660254037844387076, 1.000000000000000000, 0.8660254037844387076, 1.000000000000000000, 0.8660254037844387076, 1.000000000000000000, 0.8660254037844387076, 1.000000000000000000, 0.8660254037844387076, 1.000000000000000000, 0.8660254037844387076, 1.000000000000000000, 0.8660254037844387076, 1.000000000000000000, 0.8660254037844387076, 1.000000000000000000, 0.8660254037844387076, 1.000000000000000000, 0.8660254037844387076, 1.000000000000000000, 0.8660254037844387076, 1.000000000000000000, 0.8660254037844387076, 1.000000000000000000, 0.8660254037844387076, 1.000000000000000000, 0.8660254037844387076, 1.000000000000000000, 0.8660254037844387076, 1.000000000000000000, 0.8660254037844387076, 1.000000000000000000, 0.8660254037844387076, 1.000000000000000000, 0.8660254037844387076, 1.000000000000000000, 0.8660254037844387076, 1.000000000000000000, 0.8660254037844387076, 1.000000000000000000, 0.8660254037844387076, 1.000000000000000000, 0.8660254037844387076, 1.000000000000000000, 0.8660254037844387076, 1.000000000000000000, 0.8660254037844387076, 1.000000000000000000, 0.8660254037844387076, 1.000000000000000000, 0.8660254037844387076, 1.000000000000000000, 0.8660254037844387076, 1.000000000000000000, 0.8660254037844387076, 1.000000000000000000, 0.8660254037844387076, 1.000000000000000000, 0.8660254037844387076, 1.000000000000000000, 0.8660254037844387076, 1.000000000000000000, 0.8660254037844387076, 1.000000000000000000, 0.8660254037844387076, 1.000000000000000000, 0.8660254037844387076, 1.000000000000000000, 0.8660254037844387076, 1.000000000000000000, 0.8660254037844387076, 1.000000000000000000, 0.9111410165655264848, 0.9401539157124900736, 0.9401539157124900736, 0.9401539157124900736) ) ) 
 REPRESENTATION_ITEM ( '' )  SURFACE ( )  );
#3280 = FACE_OUTER_BOUND ( 'NONE', #14173, .T. ) ;
#3281 = ORIENTED_EDGE ( 'NONE', *, *, #14640, .T. ) ;
#3282 = CARTESIAN_POINT ( 'NONE',  ( -82.39999999999999147, -31.46250000000000568, -103.4641016151377499 ) ) ;
#3283 = CARTESIAN_POINT ( 'NONE',  ( 244.7999999999999545, -29.80000000000001492, -97.80000000000002558 ) ) ;
#3284 = DIRECTION ( 'NONE',  ( 0.000000000000000000, -1.073081856240829182E-16, -1.000000000000000000 ) ) ;
#3285 = CARTESIAN_POINT ( 'NONE',  ( 111.5000000000000142, 12.69999999999998508, 110.0000000000000142 ) ) ;
#3286 = DIRECTION ( 'NONE',  ( 0.000000000000000000, 0.000000000000000000, -1.000000000000000000 ) ) ;
#3287 = CARTESIAN_POINT ( 'NONE',  ( 235.3564303562499447, -34.56562499938547717, 101.5914258081833879 ) ) ;
#3288 = CARTESIAN_POINT ( 'NONE',  ( -85.40000000000000568, -31.26018749875867186, 101.7320508075688679 ) ) ;
#3289 = CARTESIAN_POINT ( 'NONE',  ( -84.51155386534844638, -35.25364837475780888, 98.22820752270799005 ) ) ;
#3290 = CARTESIAN_POINT ( 'NONE',  ( 85.40000000000000568, -32.25000000000000000, 99.99999999999998579 ) ) ;
#3291 = CARTESIAN_POINT ( 'NONE',  ( 82.39999999999999147, -32.27812499938548285, 96.81714838363319586 ) ) ;
#3292 = LINE ( 'NONE', #577, #8679 ) ;
#3293 = AXIS2_PLACEMENT_3D ( 'NONE', #8549, #4164, #8840 ) ;
#3294 = EDGE_CURVE ( 'NONE', #17606, #16850, #8423, .T. ) ;
#3295 = CARTESIAN_POINT ( 'NONE',  ( -82.40000000000000568, -30.00000000000000355, -99.99999999999998579 ) ) ;
#3296 = ADVANCED_FACE ( 'NONE', ( #10089 ), #14377, .T. ) ;
#3297 = CARTESIAN_POINT ( 'NONE',  ( 82.39999999999999147, -33.65624999877096712, -96.53589838486223584 ) ) ;
#3298 = FACE_OUTER_BOUND ( 'NONE', #1573, .T. ) ;
#3299 = ORIENTED_EDGE ( 'NONE', *, *, #10930, .F. ) ;
#3300 = CARTESIAN_POINT ( 'NONE',  ( 232.5999999999999943, -34.41562499938547859, -53.18285161636690361 ) ) ;
#3301 = DIRECTION ( 'NONE',  ( 1.000000000000000000, 0.000000000000000000, 0.000000000000000000 ) ) ;
#3302 = CARTESIAN_POINT ( 'NONE',  ( 234.0999999999999375, -34.74374999877096570, 102.5980762113533018 ) ) ;
#3303 = CARTESIAN_POINT ( 'NONE',  ( 233.9782151781249411, -31.00312499938548072, -47.61286128772501769 ) ) ;
#3304 = CARTESIAN_POINT ( 'NONE',  ( -83.77821517812500929, -35.01562499938548711, 102.3871387122750889 ) ) ;
#3305 = ORIENTED_EDGE ( 'NONE', *, *, #6502, .F. ) ;
#3307 = ORIENTED_EDGE ( 'NONE', *, *, #17732, .F. ) ;
#3306 = EDGE_CURVE ( 'NONE', #10687, #6930, #3916, .T. ) ;
#3308 = CARTESIAN_POINT ( 'NONE',  ( 4.082498951862918446, 2.020725942163685840, -3.500000000000001332 ) ) ;
#3309 = AXIS2_PLACEMENT_3D ( 'NONE', #14269, #718, #13985 ) ;
#3310 = DIRECTION ( 'NONE',  ( -0.000000000000000000, -1.000000000000000000, -0.000000000000000000 ) ) ;
#3311 = ORIENTED_EDGE ( 'NONE', *, *, #13489, .T. ) ;
#3312 = CARTESIAN_POINT ( 'NONE',  ( -4.000000000000000888, 1.563622288139195238, -0.2253451193528307472 ) ) ;
#3313 = CARTESIAN_POINT ( 'NONE',  ( -1.149515148933674504E-15, -4.647091401871393579, -3.572172305156879890 ) ) ;
#3314 = CARTESIAN_POINT ( 'NONE',  ( -80.90000000000000568, -33.75000000000000000, 97.40192378864668399 ) ) ;
#3315 = CARTESIAN_POINT ( 'NONE',  ( -83.90000000000000568, -34.12500000000000000, 97.40192378864668399 ) ) ;
#3316 =( BOUNDED_CURVE ( )  B_SPLINE_CURVE ( 2, ( #6775, #2360, #3823, #18593, #9696, #7051, #5409, #18696, #14371 ),
 .UNSPECIFIED., .F., .T. ) 
 B_SPLINE_CURVE_WITH_KNOTS ( ( 3, 2, 2, 2, 3 ),
 ( 0.6458333333333333703, 0.6527777777777777901, 0.6666666666666666297, 0.6805555555555555802, 0.6875000000000000000 ),
 .UNSPECIFIED. ) 
 CURVE ( )  GEOMETRIC_REPRESENTATION_ITEM ( )  RATIONAL_B_SPLINE_CURVE ( ( 0.9330127018922192983, 0.9330127018922198534, 1.000000000000000000, 0.8660254037844387076, 1.000000000000000000, 0.8660254037844387076, 1.000000000000000000, 0.9330127018922194093, 0.9330127018922194093 ) ) 
 REPRESENTATION_ITEM ( '' )  );
#3317 = CARTESIAN_POINT ( 'NONE',  ( -80.90000000000000568, -33.39374999877097139, 102.5980762113533018 ) ) ;
#3318 = DIRECTION ( 'NONE',  ( -1.000000000000000000, 4.625929269271485791E-17, 1.459037836657010301E-31 ) ) ;
#3319 = CARTESIAN_POINT ( 'NONE',  ( 4.030867648404801606, 3.732851566702016122, 0.5345114293586211707 ) ) ;
#3320 = CARTESIAN_POINT ( 'NONE',  ( 4.000000000000000000, 0.000000000000000000, 0.000000000000000000 ) ) ;
#3321 = CARTESIAN_POINT ( 'NONE',  ( 235.3564303562499447, -32.65312499938547575, 101.5914258081833879 ) ) ;
#3322 = ORIENTED_EDGE ( 'NONE', *, *, #16294, .T. ) ;
#3323 = APPLICATION_CONTEXT ( 'automotive_design' ) ;
#3324 = CARTESIAN_POINT ( 'NONE',  ( -85.15643035624999868, -32.42812499938548854, -101.5914258081833879 ) ) ;
#3325 = DIRECTION ( 'NONE',  ( 0.000000000000000000, 1.000000000000000000, 0.000000000000000000 ) ) ;
#3326 = ORIENTED_EDGE ( 'NONE', *, *, #6826, .F. ) ;
#3327 = CARTESIAN_POINT ( 'NONE',  ( -81.59615242270665192, -33.28259618943233278, -103.0000000000000000 ) ) ;
#3328 = DIRECTION ( 'NONE',  ( -1.000000000000000000, 0.000000000000000000, 0.000000000000000000 ) ) ;
#3329 = CARTESIAN_POINT ( 'NONE',  ( 4.000000000000000888, 1.563622288139206118, -0.2253451193528334950 ) ) ;
#3330 = CARTESIAN_POINT ( 'NONE',  ( 235.3564303562499447, -34.41562499938547859, -50.00000000000011369 ) ) ;
#3331 = CARTESIAN_POINT ( 'NONE',  ( -80.90000000000000568, -30.15000000000000213, 97.40192378864668399 ) ) ;
#3332 = ORIENTED_EDGE ( 'NONE', *, *, #5431, .T. ) ;
#3333 = ORIENTED_EDGE ( 'NONE', *, *, #5566, .T. ) ;
#3334 = DIRECTION ( 'NONE',  ( 1.000000000000000000, 0.000000000000000000, 0.000000000000000000 ) ) ;
#3335 = CARTESIAN_POINT ( 'NONE',  ( 83.90000000000000568, -30.52500000000000213, -97.40192378864668399 ) ) ;
#3336 = VECTOR ( 'NONE', #11034, 1000.000000000000000 ) ;
#3337 = CARTESIAN_POINT ( 'NONE',  ( -85.15643035625001289, -30.25312499938548783, 99.99999999999998579 ) ) ;
#3338 = CARTESIAN_POINT ( 'NONE',  ( 85.40000000000000568, -31.80000000000000071, 99.99999999999998579 ) ) ;
#3339 = CARTESIAN_POINT ( 'NONE',  ( -4.101948962586059011, 2.368261337751163875, -3.681124513963739187 ) ) ;
#3340 = CARTESIAN_POINT ( 'NONE',  ( 229.8435696437499871, -35.05312499938547433, 101.5914258081833879 ) ) ;
#3341 = CARTESIAN_POINT ( 'NONE',  ( 82.39999999999999147, -32.61562499938548854, -96.81714838363319586 ) ) ;
#3342 = EDGE_CURVE ( 'NONE', #12012, #4621, #15855, .T. ) ;
#3343 =( GEOMETRIC_REPRESENTATION_CONTEXT ( 3 ) GLOBAL_UNCERTAINTY_ASSIGNED_CONTEXT ( ( #9790 ) ) GLOBAL_UNIT_ASSIGNED_CONTEXT ( ( #9330, #7871, #18335 ) ) REPRESENTATION_CONTEXT ( 'NONE', 'WORKASPACE' ) );
#3344 = FACE_OUTER_BOUND ( 'NONE', #6841, .T. ) ;
#3345 = ADVANCED_FACE ( 'NONE', ( #17903 ), #2852, .T. ) ;
#3346 = CARTESIAN_POINT ( 'NONE',  ( 79.64356964375001269, -34.00312499938549138, -101.5914258081833879 ) ) ;
#3347 = ORIENTED_EDGE ( 'NONE', *, *, #404, .F. ) ;
#3348 = CARTESIAN_POINT ( 'NONE',  ( 232.5999999999999375, -33.71249999999999147, -53.46410161513786363 ) ) ;
#3349 = CARTESIAN_POINT ( 'NONE',  ( -83.90000000000000568, -34.57500000000000284, 97.40192378864668399 ) ) ;
#3350 = AXIS2_PLACEMENT_3D ( 'NONE', #13629, #10417, #11978 ) ;
#3351 =( BOUNDED_SURFACE ( )  B_SPLINE_SURFACE ( 3, 2, ( 
 ( #13920, #6412, #5047 ),
 ( #2203, #16670, #4854 ),
 ( #559, #3378, #9528 ),
 ( #10989, #5141, #10799 ),
 ( #8067, #18427, #15494 ),
 ( #15595, #18623, #2107 ) ),
 .UNSPECIFIED., .F., .F., .F. ) 
 B_SPLINE_SURFACE_WITH_KNOTS ( ( 4, 2, 4 ),
 ( 3, 3 ),
 ( 0.01651999345535507327, 0.01858032176739836741, 0.02064065007944166155 ),
 ( 0.000000000000000000, 1.000000000000000000 ),
 .UNSPECIFIED. ) 
 GEOMETRIC_REPRESENTATION_ITEM ( )  RATIONAL_B_SPLINE_SURFACE ( (
 ( 1.000000000000000000, 0.8047781103519393575, 1.000000000000000000),
 ( 1.000000000000000000, 0.8123785825613525358, 1.000000000000000000),
 ( 1.000000000000000000, 0.8190671539776085419, 1.000000000000000000),
 ( 1.000000000000000000, 0.8192352254847058424, 1.000000000000000000),
 ( 1.000000000000000000, 0.8126129677202444945, 1.000000000000000000),
 ( 1.000000000000000000, 0.8047712537969730073, 1.000000000000000000) ) ) 
 REPRESENTATION_ITEM ( '' )  SURFACE ( )  );
#3352 = CARTESIAN_POINT ( 'NONE',  ( 83.90000000000000568, -33.46874999877096712, -102.5980762113533018 ) ) ;
#3353 = UNCERTAINTY_MEASURE_WITH_UNIT (LENGTH_MEASURE( 1.000000000000000082E-05 ), #9798, 'distance_accuracy_value', 'NONE');
#3354 = DIRECTION ( 'NONE',  ( -0.000000000000000000, -1.000000000000000000, -0.000000000000000000 ) ) ;
#3355 = CARTESIAN_POINT ( 'NONE',  ( -79.64356964375001269, -30.51562499938548711, 101.5914258081833879 ) ) ;
#3356 = CARTESIAN_POINT ( 'NONE',  ( 229.8435696437499303, -34.30312499938548143, -50.00000000000011369 ) ) ;
#3357 = CARTESIAN_POINT ( 'NONE',  ( -80.90000000000000568, -31.20000000000000284, 102.5980762113533018 ) ) ;
#3358 = ORIENTED_EDGE ( 'NONE', *, *, #4450, .T. ) ;
#3359 = CARTESIAN_POINT ( 'NONE',  ( 109.9999999999999432, -29.80000000000003268, -130.0000000000000000 ) ) ;
#3360 = VECTOR ( 'NONE', #6757, 1000.000000000000000 ) ;
#3361 = CARTESIAN_POINT ( 'NONE',  ( 233.9782151781249411, -34.49062499938548143, 102.3871387122750889 ) ) ;
#3362 = CARTESIAN_POINT ( 'NONE',  ( 79.64356964375001269, -31.22812499938548925, 101.5914258081833879 ) ) ;
#3363 = AXIS2_PLACEMENT_3D ( 'NONE', #17741, #10592, #17636 ) ;
#3364 = ADVANCED_FACE ( 'NONE', ( #7630 ), #18024, .F. ) ;
#3365 = B_SPLINE_CURVE_WITH_KNOTS ( 'NONE', 3,
 ( #18436, #8075, #8172, #12858, #6614, #18828, #11391, #18632, #5056, #2117 ),
 .UNSPECIFIED., .F., .F.,
 ( 4, 2, 2, 2, 4 ),
 ( 0.3612006186103786654, 0.3925526867148934063, 0.4239047548194081472, 0.4552568229239228881, 0.4866088910284376290 ),
 .UNSPECIFIED. ) ;
#3366 = CIRCLE ( 'NONE', #11792, 5.200000000000009948 ) ;
#3367 = CARTESIAN_POINT ( 'NONE',  ( 84.28136653320187577, -32.00000000000000000, -97.98546077809228905 ) ) ;
#3368 = CARTESIAN_POINT ( 'NONE',  ( -79.64356964374998427, -30.89062499938548711, 98.40857419181659793 ) ) ;
#3369 = CARTESIAN_POINT ( 'NONE',  ( 4.630153689607048761, 6.577590292450083844E-16, 5.371010071662833063 ) ) ;
#3370 = CARTESIAN_POINT ( 'NONE',  ( 83.77821517812500929, -30.96562499938548640, 97.61286128772489690 ) ) ;
#3371 = CARTESIAN_POINT ( 'NONE',  ( 83.77821517812500929, -31.52812499938548996, -102.3871387122750889 ) ) ;
#3372 = CARTESIAN_POINT ( 'NONE',  ( 235.3564303562499447, -31.67812499938547788, -51.59142580818350865 ) ) ;
#3373 = CARTESIAN_POINT ( 'NONE',  ( -85.15643035625001289, -32.95312499938548711, 99.99999999999998579 ) ) ;
#3374 = CARTESIAN_POINT ( 'NONE',  ( -79.64356964375001269, -32.69062499938548427, -101.5914258081833879 ) ) ;
#3375 = PRODUCT_DEFINITION_CONTEXT ( 'detailed design', #1223, 'design' ) ;
#3376 = VERTEX_POINT ( 'NONE', #3041 ) ;
#3377 = CARTESIAN_POINT ( 'NONE',  ( 85.15643035624999868, -30.74062499938548143, 101.5914258081833879 ) ) ;
#3378 = CARTESIAN_POINT ( 'NONE',  ( 3.950241966888159428, -2.668221755852938415, -2.378504353001738902 ) ) ;
#3379 = VECTOR ( 'NONE', #5505, 1000.000000000000000 ) ;
#3380 = CARTESIAN_POINT ( 'NONE',  ( 4.158413352280809328, -2.044871626972829759, -3.541821552872960854 ) ) ;
#3381 = EDGE_CURVE ( 'NONE', #15492, #13429, #10568, .T. ) ;
#3382 = CARTESIAN_POINT ( 'NONE',  ( -81.02178482187500208, -33.10312499938548569, 97.61286128772489690 ) ) ;
#3383 = CARTESIAN_POINT ( 'NONE',  ( 105.1999999999999886, -4.999999999999993783, -103.0000000000000995 ) ) ;
#3384 = ORIENTED_EDGE ( 'NONE', *, *, #11545, .F. ) ;
#3385 = CARTESIAN_POINT ( 'NONE',  ( -79.39999999999999147, -30.67500000000000071, -99.99999999999998579 ) ) ;
#3386 = CARTESIAN_POINT ( 'NONE',  ( 79.39999999999999147, -34.72500000000000142, -99.99999999999998579 ) ) ;
#3387 = CARTESIAN_POINT ( 'NONE',  ( 5.599999999999998757, 0.000000000000000000, 5.200000000000001066 ) ) ;
#3388 = CARTESIAN_POINT ( 'NONE',  ( -82.39999999999999147, -34.64062499938548711, -96.81714838363319586 ) ) ;
#3389 = CARTESIAN_POINT ( 'NONE',  ( 234.0999999999999375, -32.94374999877096144, -47.40192378864679768 ) ) ;
#3390 = EDGE_CURVE ( 'NONE', #14362, #14762, #19288, .T. ) ;
#3391 = CARTESIAN_POINT ( 'NONE',  ( 235.3564303562499447, -33.66562499938548569, 101.5914258081833879 ) ) ;
#3392 = CARTESIAN_POINT ( 'NONE',  ( -85.40000000000000568, -33.09768749875867400, 99.99999999999998579 ) ) ;
#3393 = ORIENTED_EDGE ( 'NONE', *, *, #8869, .T. ) ;
#3394 = CARTESIAN_POINT ( 'NONE',  ( 99.99999999999994316, -21.80000000000003268, -137.3499999999999943 ) ) ;
#3395 = CARTESIAN_POINT ( 'NONE',  ( 109.9999999999999574, -21.80000000000003268, -137.3499999999999943 ) ) ;
#3396 = CARTESIAN_POINT ( 'NONE',  ( 83.77821517812500929, -34.56562499938548427, 97.61286128772489690 ) ) ;
#3397 = DIRECTION ( 'NONE',  ( -0.000000000000000000, -1.000000000000000000, -0.000000000000000000 ) ) ;
#3398 = CARTESIAN_POINT ( 'NONE',  ( 105.5000000000000142, 12.69999999999998508, 30.20101012677667285 ) ) ;
#3399 = CARTESIAN_POINT ( 'NONE',  ( 79.64356964374999848, -31.37812499938548427, -99.99999999999998579 ) ) ;
#3400 = PLANE ( 'NONE',  #15847 ) ;
#3401 = ORIENTED_EDGE ( 'NONE', *, *, #10471, .T. ) ;
#3402 = CARTESIAN_POINT ( 'NONE',  ( 229.8435696437499587, -32.54062499938547859, -51.59142580818350154 ) ) ;
#3403 = CARTESIAN_POINT ( 'NONE',  ( 115.5999999999999517, -21.80000000000002913, -140.0000000000000000 ) ) ;
#3404 = CARTESIAN_POINT ( 'NONE',  ( 235.3564303562499447, -31.37812499938547717, 99.99999999999998579 ) ) ;
#3405 = CARTESIAN_POINT ( 'NONE',  ( 229.5999999999999375, -34.89374999877096428, -50.00000000000011369 ) ) ;
#3406 = CARTESIAN_POINT ( 'NONE',  ( -81.02178482187500208, -34.94062499938548427, 102.3871387122750889 ) ) ;
#3407 = ORIENTED_EDGE ( 'NONE', *, *, #3262, .F. ) ;
#3408 = EDGE_LOOP ( 'NONE', ( #5079, #441, #8494, #13671 ) ) ;
#3409 = CARTESIAN_POINT ( 'NONE',  ( -80.24181665645332373, -32.00000000000000711, 97.97695283456452842 ) ) ;
#3410 =( BOUNDED_CURVE ( )  B_SPLINE_CURVE ( 2, ( #1524, #11866, #17834, #61, #18224, #6015, #1798, #9126, #11961 ),
 .UNSPECIFIED., .F., .F. ) 
 B_SPLINE_CURVE_WITH_KNOTS ( ( 3, 2, 2, 2, 3 ),
 ( 0.1041666666666666713, 0.1111111111111111049, 0.1250000000000000000, 0.1388888888888888951, 0.1458333333333334814 ),
 .UNSPECIFIED. ) 
 CURVE ( )  GEOMETRIC_REPRESENTATION_ITEM ( )  RATIONAL_B_SPLINE_CURVE ( ( 0.9330127018922194093, 0.9330127018922194093, 1.000000000000000000, 0.8660254037844387076, 1.000000000000000000, 0.8660254037844387076, 1.000000000000000000, 0.9330127018922180770, 0.9330127018922194093 ) ) 
 REPRESENTATION_ITEM ( '' )  );
#3411 = FACE_OUTER_BOUND ( 'NONE', #1796, .T. ) ;
#3412 = CARTESIAN_POINT ( 'NONE',  ( -82.40000000000001990, -34.16250000000000853, -103.0000000000000000 ) ) ;
#3413 = VERTEX_POINT ( 'NONE', #1585 ) ;
#3414 = CARTESIAN_POINT ( 'NONE',  ( -4.000000000000000000, 1.941961291383472732, -0.3515519931180205448 ) ) ;
#3415 = CARTESIAN_POINT ( 'NONE',  ( -83.90000000000000568, -34.51874999877097139, -102.5980762113533018 ) ) ;
#3416 = CARTESIAN_POINT ( 'NONE',  ( -82.39999999999999147, -34.16250000000000142, 97.00000000000000000 ) ) ;
#3417 = CARTESIAN_POINT ( 'NONE',  ( -80.90000000000000568, -31.59374999877097423, 102.5980762113533018 ) ) ;
#3418 = CARTESIAN_POINT ( 'NONE',  ( -82.39999999999999147, -33.43124999877097281, 103.4641016151377499 ) ) ;
#3419 = CARTESIAN_POINT ( 'NONE',  ( 85.16220480609065646, -34.99999999999999289, -98.91314642826793602 ) ) ;
#3420 = CARTESIAN_POINT ( 'NONE',  ( 231.3931070460713499, -35.00000000000000000, 97.24646917567284277 ) ) ;
#3421 = EDGE_CURVE ( 'NONE', #12300, #13090, #7280, .T. ) ;
#3422 = DIRECTION ( 'NONE',  ( 0.000000000000000000, 1.000000000000000000, 0.000000000000000000 ) ) ;
#3423 = FACE_OUTER_BOUND ( 'NONE', #14442, .T. ) ;
#3424 = CARTESIAN_POINT ( 'NONE',  ( 229.8435696437499303, -35.09062499938547575, 99.99999999999998579 ) ) ;
#3425 = CARTESIAN_POINT ( 'NONE',  ( 229.8435696437499871, -31.90312499938547575, 101.5914258081833879 ) ) ;
#3426 = ORIENTED_EDGE ( 'NONE', *, *, #8204, .F. ) ;
#3427 = CARTESIAN_POINT ( 'NONE',  ( 231.0999999999999375, -31.66874999877096641, 102.5980762113533018 ) ) ;
#3428 = CARTESIAN_POINT ( 'NONE',  ( 4.093692494532767512, 4.043567292011554848, -1.127116027090594736E-16 ) ) ;
#3429 = ORIENTED_EDGE ( 'NONE', *, *, #16643, .F. ) ;
#3430 = CARTESIAN_POINT ( 'NONE',  ( 82.40000000000000568, -30.00000000000000355, 103.0000000000000000 ) ) ;
#3431 = CARTESIAN_POINT ( 'NONE',  ( 82.49978216248241836, -35.00000000000000711, -102.7603866155199910 ) ) ;
#3432 = CARTESIAN_POINT ( 'NONE',  ( 82.40000000000000568, -33.03750000000000142, -102.9999999999999858 ) ) ;
#3433 = VERTEX_POINT ( 'NONE', #132 ) ;
#3434 = CARTESIAN_POINT ( 'NONE',  ( 231.0999999999999375, -33.46874999877096002, 102.5980762113533018 ) ) ;
#3435 = EDGE_LOOP ( 'NONE', ( #8036, #5423, #6861, #10062 ) ) ;
#3436 = ORIENTED_EDGE ( 'NONE', *, *, #7205, .F. ) ;
#3437 =( BOUNDED_CURVE ( )  B_SPLINE_CURVE ( 2, ( #11845, #17813, #10190, #7256, #10577, #17720, #8907, #12037, #4623 ),
 .UNSPECIFIED., .F., .F. ) 
 B_SPLINE_CURVE_WITH_KNOTS ( ( 3, 2, 2, 2, 3 ),
 ( 0.3125000000000001110, 0.3194444444444444198, 0.3333333333333333148, 0.3472222222222222099, 0.3541666666666666852 ),
 .UNSPECIFIED. ) 
 CURVE ( )  GEOMETRIC_REPRESENTATION_ITEM ( )  RATIONAL_B_SPLINE_CURVE ( ( 0.9330127018922194093, 0.9330127018922204085, 1.000000000000000000, 0.8660254037844387076, 1.000000000000000000, 0.8660254037844387076, 1.000000000000000000, 0.9330127018922190762, 0.9330127018922194093 ) ) 
 REPRESENTATION_ITEM ( '' )  );
#3438 = CARTESIAN_POINT ( 'NONE',  ( -82.15584532983329780, -32.00000000000000000, 102.8696726379688329 ) ) ;
#3439 = CARTESIAN_POINT ( 'NONE',  ( 82.39999999999999147, -30.33750000000000213, -103.4641016151377499 ) ) ;
#3440 = CARTESIAN_POINT ( 'NONE',  ( 232.5999999999999375, -29.99999999999999645, -50.00000000000011369 ) ) ;
#3441 = CARTESIAN_POINT ( 'NONE',  ( -80.90000000000000568, -34.74374999877097281, 102.5980762113533018 ) ) ;
#3442 = CARTESIAN_POINT ( 'NONE',  ( -82.40000000000000568, -30.00000000000000355, 103.0000000000000000 ) ) ;
#3443 = CARTESIAN_POINT ( 'NONE',  ( 81.59615242270662350, -33.22634618820330843, 102.9999999999999858 ) ) ;
#3444 = CARTESIAN_POINT ( 'NONE',  ( 83.77821517812500929, -33.77812499938548285, -102.3871387122750889 ) ) ;
#3445 = CARTESIAN_POINT ( 'NONE',  ( 81.90908125315206689, -31.99999999999999289, -97.16185054499327123 ) ) ;
#3446 = CARTESIAN_POINT ( 'NONE',  ( -81.02178482187500208, -32.54062499938548569, 97.61286128772489690 ) ) ;
#3447 = CARTESIAN_POINT ( 'NONE',  ( 81.02178482187500208, -34.34062499938548285, -97.61286128772489690 ) ) ;
#3448 = ORIENTED_EDGE ( 'NONE', *, *, #18470, .F. ) ;
#3449 = CARTESIAN_POINT ( 'NONE',  ( 231.0999999999999375, -32.32499999999999574, -52.59807621135342970 ) ) ;
#3450 = CARTESIAN_POINT ( 'NONE',  ( 229.8435696437499587, -32.91562499938547859, 101.5914258081833879 ) ) ;
#3451 = CARTESIAN_POINT ( 'NONE',  ( -83.77821517812500929, -32.57812499938548711, 97.61286128772489690 ) ) ;
#3452 = CARTESIAN_POINT ( 'NONE',  ( 231.2217848218749339, -33.47812499938547859, -52.38713871227520968 ) ) ;
#3453 = CARTESIAN_POINT ( 'NONE',  ( -82.39999999999999147, -31.91250000000000497, 96.53589838486223584 ) ) ;
#3454 = ORIENTED_EDGE ( 'NONE', *, *, #2503, .F. ) ;
#3455 = CARTESIAN_POINT ( 'NONE',  ( -85.00132729414809774, -35.00000000000000000, 101.2112556745012881 ) ) ;
#3456 = CARTESIAN_POINT ( 'NONE',  ( 82.32247963938024782, -34.99999999999998579, 97.23891671615865562 ) ) ;
#3457 = CARTESIAN_POINT ( 'NONE',  ( 82.39999999999999147, -31.82812499938548356, 96.81714838363319586 ) ) ;
#3458 = CARTESIAN_POINT ( 'NONE',  ( 83.90000000000000568, -32.56874999877096855, -102.5980762113533018 ) ) ;
#3459 = CARTESIAN_POINT ( 'NONE',  ( -79.64356964374998427, -30.96562499938548640, 101.5914258081833879 ) ) ;
#3460 = CARTESIAN_POINT ( 'NONE',  ( 79.79666399293472523, -31.99999999999999289, 98.51078102784474311 ) ) ;
#3461 = CARTESIAN_POINT ( 'NONE',  ( 83.77821517812500929, -34.37812499938548427, 102.3871387122750889 ) ) ;
#3462 =( BOUNDED_CURVE ( )  B_SPLINE_CURVE ( 3, ( #2535, #18583, #14359, #5396 ),
 .UNSPECIFIED., .F., .F. ) 
 B_SPLINE_CURVE_WITH_KNOTS ( ( 4, 4 ),
 ( 1.538098430149248408, 2.146777830243033147 ),
 .UNSPECIFIED. ) 
 CURVE ( )  GEOMETRIC_REPRESENTATION_ITEM ( )  RATIONAL_B_SPLINE_CURVE ( ( 1.000000000000000000, 0.9693633521240627715, 0.9693633521240627715, 1.000000000000000000 ) ) 
 REPRESENTATION_ITEM ( '' )  );
#3463 = CARTESIAN_POINT ( 'NONE',  ( 82.39999999999999147, -30.81562499938548427, -96.81714838363319586 ) ) ;
#3464 = CARTESIAN_POINT ( 'NONE',  ( 231.2217848218749339, -31.41562499938547859, -47.61286128772501769 ) ) ;
#3465 = CARTESIAN_POINT ( 'NONE',  ( -79.64356964374999848, -33.17812499938548854, 99.99999999999998579 ) ) ;
#3466 = CARTESIAN_POINT ( 'NONE',  ( -79.64356964374999848, -32.72812499938548569, -99.99999999999998579 ) ) ;
#3467 = EDGE_CURVE ( 'NONE', #15949, #16690, #12639, .T. ) ;
#3468 = ORIENTED_EDGE ( 'NONE', *, *, #10593, .F. ) ;
#3469 = CARTESIAN_POINT ( 'NONE',  ( 83.77821517812500929, -33.77812499938548285, 97.61286128772489690 ) ) ;
#3470 = CARTESIAN_POINT ( 'NONE',  ( 229.5999999999999375, -32.21249999999999858, 101.7320508075688821 ) ) ;
#3471 = CARTESIAN_POINT ( 'NONE',  ( -79.64356964375001269, -31.30312499938548854, 101.5914258081833879 ) ) ;
#3472 = CARTESIAN_POINT ( 'NONE',  ( -82.39999999999999147, -33.74062499938548854, 103.1828516163667899 ) ) ;
#3473 = CARTESIAN_POINT ( 'NONE',  ( 83.90000000000000568, -33.01874999877097139, 97.40192378864668399 ) ) ;
#3474 = ORIENTED_EDGE ( 'NONE', *, *, #2828, .T. ) ;
#3475 = CARTESIAN_POINT ( 'NONE',  ( -79.39999999999999147, -33.82500000000000284, -99.99999999999998579 ) ) ;
#3476 = DIRECTION ( 'NONE',  ( 1.000000000000000000, 0.000000000000000000, 0.000000000000000000 ) ) ;
#3477 = CARTESIAN_POINT ( 'NONE',  ( 82.39999999999999147, -33.65624999877097423, 103.0000000000000000 ) ) ;
#3478 = FACE_OUTER_BOUND ( 'NONE', #6668, .T. ) ;
#3479 = CARTESIAN_POINT ( 'NONE',  ( 229.8435696437499871, -30.17812499938547433, 98.40857419181659793 ) ) ;
#3480 = CARTESIAN_POINT ( 'NONE',  ( -83.90000000000000568, -33.17268749875866973, 97.40192378864668399 ) ) ;
#3481 = EDGE_LOOP ( 'NONE', ( #16334, #11188, #3151, #9045 ) ) ;
#3482 = CARTESIAN_POINT ( 'NONE',  ( 111.0000000000000000, 6.932050807568743700, -145.0319487353994532 ) ) ;
#3483 = CARTESIAN_POINT ( 'NONE',  ( -85.40000000000000568, -34.44374999877096855, 99.99999999999998579 ) ) ;
#3484 = CARTESIAN_POINT ( 'NONE',  ( 99.99999999999994316, -29.80000000000000782, -150.0000000000000000 ) ) ;
#3485 = LINE ( 'NONE', #1833, #2453 ) ;
#3486 = CYLINDRICAL_SURFACE ( 'NONE', #15828, 3.000000000000002665 ) ;
#3487 = CARTESIAN_POINT ( 'NONE',  ( 85.15643035624999868, -32.54062499938548569, -98.40857419181659793 ) ) ;
#3488 = CARTESIAN_POINT ( 'NONE',  ( 4.071447262713887127, 2.020725942163688504, 3.500000000000000000 ) ) ;
#3489 = EDGE_CURVE ( 'NONE', #4350, #7254, #1488, .T. ) ;
#3490=STYLED_ITEM('',(#19371),#1092);
#3491 = VERTEX_POINT ( 'NONE', #12415 ) ;
#3492 = CARTESIAN_POINT ( 'NONE',  ( 235.3564303562499447, -34.94062499938547717, -51.59142580818350154 ) ) ;
#3493 = APPLICATION_PROTOCOL_DEFINITION ( 'draft international standard', 'automotive_design', 1998, #1223 ) ;
#3494 = CARTESIAN_POINT ( 'NONE',  ( 231.2217848218749339, -31.52812499938548285, 102.3871387122750889 ) ) ;
#3495 = CARTESIAN_POINT ( 'NONE',  ( 235.3564303562499447, -31.37812499938547717, -50.00000000000011369 ) ) ;
#3496 = EDGE_CURVE ( 'NONE', #3020, #14066, #11714, .T. ) ;
#3497 = CARTESIAN_POINT ( 'NONE',  ( -85.15643035625001289, -32.39062499938548711, 99.99999999999998579 ) ) ;
#3498 = CARTESIAN_POINT ( 'NONE',  ( 3.951447005078452701, 3.704664227300100698, -0.5833333333333330373 ) ) ;
#3499 = ORIENTED_EDGE ( 'NONE', *, *, #9854, .T. ) ;
#3500 = ORIENTED_EDGE ( 'NONE', *, *, #19165, .F. ) ;
#3501 = CARTESIAN_POINT ( 'NONE',  ( 232.5999999999999375, -32.75624999877096144, -53.00000000000010658 ) ) ;
#3502 = CARTESIAN_POINT ( 'NONE',  ( -83.90000000000000568, -30.91874999877096997, 97.40192378864668399 ) ) ;
#3503 = DIRECTION ( 'NONE',  ( 0.000000000000000000, -0.000000000000000000, -1.000000000000000000 ) ) ;
#3504 = EDGE_LOOP ( 'NONE', ( #8592, #11763, #310, #18188 ) ) ;
#3505 = CARTESIAN_POINT ( 'NONE',  ( -4.000000000000000000, 2.309401076758498483, -0.4999999999999927280 ) ) ;
#3506 = CARTESIAN_POINT ( 'NONE',  ( -79.39999999999999147, -33.28124999877096712, -101.7320508075688821 ) ) ;
#3507 = AXIS2_PLACEMENT_3D ( 'NONE', #9368, #313, #6452 ) ;
#3508 = VECTOR ( 'NONE', #8111, 1000.000000000000000 ) ;
#3509 = DIRECTION ( 'NONE',  ( -0.000000000000000000, -1.000000000000000000, -0.000000000000000000 ) ) ;
#3510 = CARTESIAN_POINT ( 'NONE',  ( -85.40000000000000568, -31.25624999877096855, 101.7320508075688679 ) ) ;
#3511 = CARTESIAN_POINT ( 'NONE',  ( -80.90000000000000568, -33.84374999877096712, 102.5980762113533018 ) ) ;
#3512 = DIRECTION ( 'NONE',  ( 1.000000000000000000, 0.000000000000000000, -0.000000000000000000 ) ) ;
#3513 = B_SPLINE_CURVE_WITH_KNOTS ( 'NONE', 3,
 ( #5404, #17409, #10077, #4023, #16132, #5686, #18972, #1000, #16234, #7234, #11634, #15938, #2541, #14455, #1087, #7045, #18779, #10169 ),
 .UNSPECIFIED., .F., .F.,
 ( 4, 2, 2, 2, 2, 2, 2, 2, 4 ),
 ( 0.000000000000000000, 0.0007106627595359784168, 0.001421325519071956834, 0.002131988278607935359, 0.002842651038143913667, 0.003553313797679891976, 0.004263976557215870718, 0.004974639316751849026, 0.005685302076287827334 ),
 .UNSPECIFIED. ) ;
#3514 = EDGE_CURVE ( 'NONE', #5195, #12222, #6669, .T. ) ;
#3515 = CARTESIAN_POINT ( 'NONE',  ( -79.77811200999879304, -35.00000000000000000, -99.14934632385212865 ) ) ;
#3516 = CARTESIAN_POINT ( 'NONE',  ( -79.39999999999999147, -34.25624999877096855, 101.7320508075688537 ) ) ;
#3517 = CARTESIAN_POINT ( 'NONE',  ( 233.9782151781249411, -34.04062499938547859, 102.3871387122750889 ) ) ;
#3518 = EDGE_CURVE ( 'NONE', #3491, #12219, #10847, .T. ) ;
#3519 = ORIENTED_EDGE ( 'NONE', *, *, #6542, .F. ) ;
#3520 = CARTESIAN_POINT ( 'NONE',  ( -85.15643035624999868, -34.60312499938548569, -98.40857419181659793 ) ) ;
#3521 = CARTESIAN_POINT ( 'NONE',  ( 232.5999999999999091, -32.08124999877096428, 102.9999999999999858 ) ) ;
#3522 = AXIS2_PLACEMENT_3D ( 'NONE', #3623, #5105, #6666 ) ;
#3523 =( BOUNDED_CURVE ( )  B_SPLINE_CURVE ( 2, ( #4770, #3768, #9436, #3576, #8363, #10905, #9735, #5147, #9642 ),
 .UNSPECIFIED., .F., .F. ) 
 B_SPLINE_CURVE_WITH_KNOTS ( ( 3, 2, 2, 2, 3 ),
 ( 0.3541666666666666297, 0.3611111111111111049, 0.3750000000000000000, 0.3888888888888888951, 0.3958333333333334259 ),
 .UNSPECIFIED. ) 
 CURVE ( )  GEOMETRIC_REPRESENTATION_ITEM ( )  RATIONAL_B_SPLINE_CURVE ( ( 0.9330127018922194093, 0.9330127018922190762, 1.000000000000000000, 0.8660254037844387076, 1.000000000000000000, 0.8660254037844387076, 1.000000000000000000, 0.9330127018922185211, 0.9330127018922192983 ) ) 
 REPRESENTATION_ITEM ( '' )  );
#3524 = ORIENTED_EDGE ( 'NONE', *, *, #8413, .F. ) ;
#3525 = DIRECTION ( 'NONE',  ( 1.000000000000000000, -4.625929269271494788E-16, 0.000000000000000000 ) ) ;
#3526 = CLOSED_SHELL ( 'NONE', ( #5779, #17132, #6134, #11799, #1815, #10200, #17470, #1365, #19082, #4921, #3013, #6402, #15074, #16330, #934, #7816, #3296, #10940, #3345, #18227, #18400, #9723, #17020, #2713, #650, #905, #12213, #2789, #10924, #11662, #667, #8417, #17025, #13751 ) ) ;
#3527 = PLANE ( 'NONE',  #11801 ) ;
#3528 = UNCERTAINTY_MEASURE_WITH_UNIT (LENGTH_MEASURE( 1.000000000000000082E-05 ), #13971, 'distance_accuracy_value', 'NONE');
#3529 = CARTESIAN_POINT ( 'NONE',  ( 79.39999999999999147, -32.06250000000000000, 98.26794919243113213 ) ) ;
#3530 = ORIENTED_EDGE ( 'NONE', *, *, #11184, .T. ) ;
#3531 = CYLINDRICAL_SURFACE ( 'NONE', #15707, 3.000000000000002665 ) ;
#3532 = VERTEX_POINT ( 'NONE', #15253 ) ;
#3533 = ORIENTED_EDGE ( 'NONE', *, *, #16809, .F. ) ;
#3534 = CARTESIAN_POINT ( 'NONE',  ( 80.90000000000000568, -34.59374999877096712, 102.5980762113533018 ) ) ;
#3535 = ADVANCED_FACE ( 'NONE', ( #10849, #12604, #8116 ), #13973, .F. ) ;
#3536 = CARTESIAN_POINT ( 'NONE',  ( 80.90000000000000568, -30.75000000000000355, -102.5980762113533018 ) ) ;
#3537 = CARTESIAN_POINT ( 'NONE',  ( 4.175813232069151226, -4.122719923832748101, -3.898053888241413974E-16 ) ) ;
#3538 = CARTESIAN_POINT ( 'NONE',  ( -82.39999999999999147, -35.00624999877097565, 96.53589838486223584 ) ) ;
#3539 = CARTESIAN_POINT ( 'NONE',  ( -83.20384757729338787, -32.10134618820330132, -97.00000000000000000 ) ) ;
#3540 = CARTESIAN_POINT ( 'NONE',  ( -2.171643655288372443, 3.365003104552320767, 2.541098841762897165E-18 ) ) ;
#3541 = CARTESIAN_POINT ( 'NONE',  ( 79.64356964374998427, -32.31562499938548427, -101.5914258081833879 ) ) ;
#3542 = CARTESIAN_POINT ( 'NONE',  ( -80.90000000000000568, -33.30000000000000426, 97.40192378864668399 ) ) ;
#3543 = CARTESIAN_POINT ( 'NONE',  ( -82.39999999999999147, -32.27812499938548285, 103.1828516163667899 ) ) ;
#3544 = CARTESIAN_POINT ( 'NONE',  ( 83.77821517812500929, -33.21562499938548285, -102.3871387122750889 ) ) ;
#3545 = ORIENTED_EDGE ( 'NONE', *, *, #8064, .T. ) ;
#3546 = CARTESIAN_POINT ( 'NONE',  ( 232.5999999999999375, -31.91249999999999432, -53.46410161513786363 ) ) ;
#3547 = EDGE_CURVE ( 'NONE', #4006, #18536, #1866, .T. ) ;
#3548 = CARTESIAN_POINT ( 'NONE',  ( -79.39999999999999147, -34.72500000000000142, 99.99999999999998579 ) ) ;
#3549 = CARTESIAN_POINT ( 'NONE',  ( -85.40000000000000568, -34.03124999877096712, 98.26794919243111792 ) ) ;
#3550 = CARTESIAN_POINT ( 'NONE',  ( 235.3564303562499447, -32.69062499938547717, 98.40857419181659793 ) ) ;
#3551 = CARTESIAN_POINT ( 'NONE',  ( -79.64356964374999848, -31.37812499938548427, 99.99999999999998579 ) ) ;
#3552 = CARTESIAN_POINT ( 'NONE',  ( 235.3564303562499447, -33.17812499938548143, -50.00000000000011369 ) ) ;
#3553 = CARTESIAN_POINT ( 'NONE',  ( -80.90000000000000568, -33.00000000000000000, 102.5980762113533018 ) ) ;
#3554 = EDGE_LOOP ( 'NONE', ( #6738, #7388, #9688, #4859 ) ) ;
#3555 = CARTESIAN_POINT ( 'NONE',  ( 94.79999999999984084, 0.000000000000000000, 150.0000000000000000 ) ) ;
#3556 = EDGE_CURVE ( 'NONE', #11655, #8657, #2027, .T. ) ;
#3557 = CARTESIAN_POINT ( 'NONE',  ( 81.79008970393682887, -35.00000000000001421, 97.30603528924578427 ) ) ;
#3558 = CARTESIAN_POINT ( 'NONE',  ( 85.15643035625001289, -31.49062499938548498, 99.99999999999998579 ) ) ;
#3559 = CARTESIAN_POINT ( 'NONE',  ( 235.5999999999999943, -34.68749999999999289, 98.26794919243110371 ) ) ;
#3560 = CARTESIAN_POINT ( 'NONE',  ( -85.15643035625001289, -31.56562499938548427, 101.5914258081833879 ) ) ;
#3561 = CARTESIAN_POINT ( 'NONE',  ( 79.68596062386927770, -32.00000000000000000, 98.72172371342817598 ) ) ;
#3562 = CARTESIAN_POINT ( 'NONE',  ( 79.64356964374999848, -30.36562499938548498, 99.99999999999998579 ) ) ;
#3563 = CARTESIAN_POINT ( 'NONE',  ( 79.64356964375001269, -31.41562499938548569, -101.5914258081833879 ) ) ;
#3564 = CARTESIAN_POINT ( 'NONE',  ( 231.2217848218749339, -31.56562499938547717, -52.38713871227520968 ) ) ;
#3565 = CARTESIAN_POINT ( 'NONE',  ( -85.15643035625001289, -33.44062499938548427, 98.40857419181659793 ) ) ;
#3566 = CARTESIAN_POINT ( 'NONE',  ( -85.15643035624999868, -32.46562499938548996, -98.40857419181659793 ) ) ;
#3567 = ORIENTED_EDGE ( 'NONE', *, *, #9167, .F. ) ;
#3568 = CARTESIAN_POINT ( 'NONE',  ( 79.64356964375001269, -31.79062499938548569, 101.5914258081833879 ) ) ;
#3569 = CARTESIAN_POINT ( 'NONE',  ( -2.688821387764050996E-14, -4.618802153517012954, -0.4999999999999995559 ) ) ;
#3570 = CARTESIAN_POINT ( 'NONE',  ( -85.15643035625001289, -30.14062499938548711, 99.99999999999998579 ) ) ;
#3571 = CARTESIAN_POINT ( 'NONE',  ( -85.15643035624999868, -34.79062499938548569, 98.40857419181659793 ) ) ;
#3572 = CARTESIAN_POINT ( 'NONE',  ( -0.6448876103708541807, -4.246476118072358474, -0.2256878752776773356 ) ) ;
#3573 = ORIENTED_EDGE ( 'NONE', *, *, #10096, .T. ) ;
#3574 = CARTESIAN_POINT ( 'NONE',  ( -80.90000000000000568, -33.75000000000000000, -102.5980762113533018 ) ) ;
#3575 = PRODUCT_DEFINITION_SHAPE ( 'NONE', 'NONE',  #4398 ) ;
#3576 = CARTESIAN_POINT ( 'NONE',  ( -79.39999999999999147, -32.38124999877096855, 98.26794919243110371 ) ) ;
#3577 = CARTESIAN_POINT ( 'NONE',  ( -82.40000000000000568, -30.00000000000000355, 96.99999999999998579 ) ) ;
#3578 = CARTESIAN_POINT ( 'NONE',  ( 232.5999999999999375, -33.06562499938547717, 96.81714838363319586 ) ) ;
#3579 = CARTESIAN_POINT ( 'NONE',  ( -79.39999999999999147, -35.08518749875868536, 98.26794919243110371 ) ) ;
#3580 =( REPRESENTATION_RELATIONSHIP ('NONE','NONE', #14468, #7749 ) REPRESENTATION_RELATIONSHIP_WITH_TRANSFORMATION ( #10232 )SHAPE_REPRESENTATION_RELATIONSHIP( ) );
#3581 = EDGE_LOOP ( 'NONE', ( #8099, #9700, #15443, #10797 ) ) ;
#3582 = CARTESIAN_POINT ( 'NONE',  ( -81.02178482187500208, -35.05312499938548854, 102.3871387122750889 ) ) ;
#3583 = CARTESIAN_POINT ( 'NONE',  ( -85.40000000000000568, -34.48124999877096997, 98.26794919243111792 ) ) ;
#3584 = CARTESIAN_POINT ( 'NONE',  ( 85.15643035625001289, -34.64062499938548711, 99.99999999999998579 ) ) ;
#3585 = FACE_OUTER_BOUND ( 'NONE', #1484, .T. ) ;
#3586 = CARTESIAN_POINT ( 'NONE',  ( 111.1957315586905537, 7.271067811865449926, -150.0000000000000000 ) ) ;
#3587 = CARTESIAN_POINT ( 'NONE',  ( 79.64356964375001269, -30.89062499938548711, -98.40857419181659793 ) ) ;
#3588 = CARTESIAN_POINT ( 'NONE',  ( 79.39999999999999147, -34.72500000000000142, 99.99999999999998579 ) ) ;
#3589 = ORIENTED_EDGE ( 'NONE', *, *, #16423, .F. ) ;
#3590 = CARTESIAN_POINT ( 'NONE',  ( 82.39999999999999147, -31.40624999877097068, 103.4641016151377499 ) ) ;
#3591 = APPLICATION_PROTOCOL_DEFINITION ( 'draft international standard', 'automotive_design', 1998, #8572 ) ;
#3592 = CARTESIAN_POINT ( 'NONE',  ( 233.9782151781249411, -32.65312499938548285, 97.61286128772489690 ) ) ;
#3593 = CARTESIAN_POINT ( 'NONE',  ( 235.3564303562499447, -31.82812499938547646, -50.00000000000011369 ) ) ;
#3594 = CARTESIAN_POINT ( 'NONE',  ( -81.02178482187500208, -34.34062499938548285, 97.61286128772489690 ) ) ;
#3595 = CARTESIAN_POINT ( 'NONE',  ( -79.39999999999999147, -32.88750000000000284, -101.7320508075688963 ) ) ;
#3596 = EDGE_LOOP ( 'NONE', ( #12625, #3987, #13591 ) ) ;
#3597 = ORIENTED_EDGE ( 'NONE', *, *, #12577, .F. ) ;
#3598 = CARTESIAN_POINT ( 'NONE',  ( -82.39999999999999147, -31.37812499938548427, -96.81714838363319586 ) ) ;
#3599 = CARTESIAN_POINT ( 'NONE',  ( 82.40000000000000568, -33.03750000000000142, 96.99999999999998579 ) ) ;
#3600 = ORIENTED_EDGE ( 'NONE', *, *, #4576, .F. ) ;
#3601 = CARTESIAN_POINT ( 'NONE',  ( 83.77821517812500929, -32.42812499938548854, 97.61286128772489690 ) ) ;
#3602 = CARTESIAN_POINT ( 'NONE',  ( -79.39999999999999147, -33.76874999877097139, -99.99999999999998579 ) ) ;
#3603 = VECTOR ( 'NONE', #7378, 1000.000000000000000 ) ;
#3604 = LINE ( 'NONE', #12308, #12554 ) ;
#3605 = CARTESIAN_POINT ( 'NONE',  ( -82.39999999999999147, -32.75624999877096855, 96.53589838486223584 ) ) ;
#3606 = CARTESIAN_POINT ( 'NONE',  ( -82.39999999999999147, -32.98124999877096997, 103.4641016151377499 ) ) ;
#3607 = CARTESIAN_POINT ( 'NONE',  ( -83.90000000000000568, -32.32500000000000284, 97.40192378864668399 ) ) ;
#3608 = EDGE_CURVE ( 'NONE', #10334, #4020, #706, .T. ) ;
#3609 = EDGE_CURVE ( 'NONE', #6906, #6376, #16464, .T. ) ;
#3610 = CARTESIAN_POINT ( 'NONE',  ( 81.59615242270662350, -34.31115380933863435, -102.9999999999999716 ) ) ;
#3611 = CARTESIAN_POINT ( 'NONE',  ( 233.9825576637930169, -32.00000000000000000, 102.5835086888314294 ) ) ;
#3612 = CARTESIAN_POINT ( 'NONE',  ( 233.9782151781249411, -34.49062499938548143, 102.3871387122750889 ) ) ;
#3613 = EDGE_LOOP ( 'NONE', ( #2473, #9269, #13788, #9361 ) ) ;
#3614 = CARTESIAN_POINT ( 'NONE',  ( 79.64356964374998427, -32.20312499938548711, -101.5914258081833879 ) ) ;
#3615 = CARTESIAN_POINT ( 'NONE',  ( -81.02178482187500208, -34.49062499938548854, -97.61286128772489690 ) ) ;
#3616 = DIRECTION ( 'NONE',  ( 1.000000000000000000, 0.000000000000000000, 0.000000000000000000 ) ) ;
#3617 = VERTEX_POINT ( 'NONE', #7825 ) ;
#3618 = VECTOR ( 'NONE', #8272, 1000.000000000000000 ) ;
#3619 = CARTESIAN_POINT ( 'NONE',  ( -79.39999999999999147, -33.33749999999999858, -101.7320508075688963 ) ) ;
#3620 = CARTESIAN_POINT ( 'NONE',  ( 0.6507732100473444525, -4.243078065514795050, -0.2236248678334952777 ) ) ;
#3621 = CARTESIAN_POINT ( 'NONE',  ( -82.39999999999999147, -33.26250000000000284, 96.53589838486223584 ) ) ;
#3622 = ORIENTED_EDGE ( 'NONE', *, *, #10828, .T. ) ;
#3623 = CARTESIAN_POINT ( 'NONE',  ( 0.000000000000000000, 0.000000000000000000, 0.000000000000000000 ) ) ;
#3625 = EDGE_CURVE ( 'NONE', #10188, #1583, #9378, .T. ) ;
#3624 = CARTESIAN_POINT ( 'NONE',  ( 230.7186334667983658, -32.00000000000000711, 97.98546077809203325 ) ) ;
#3626 = ORIENTED_EDGE ( 'NONE', *, *, #1534, .F. ) ;
#3627 = CARTESIAN_POINT ( 'NONE',  ( 79.39999999999999147, -34.66874999877096997, 99.99999999999998579 ) ) ;
#3628 = CARTESIAN_POINT ( 'NONE',  ( 82.39999999999999147, -34.52812499938548996, -103.1828516163667899 ) ) ;
#3629 = CARTESIAN_POINT ( 'NONE',  ( 3.972709601346593011, -2.746729940827192795, 2.374099244652734697 ) ) ;
#3630 = COLOUR_RGB ( '',1.000000000000000000, 0.9490196078431372140, 0.9098039215686274384 ) ;
#3631 = CARTESIAN_POINT ( 'NONE',  ( -79.39999999999999147, -34.66874999877096997, 99.99999999999998579 ) ) ;
#3632 = CARTESIAN_POINT ( 'NONE',  ( -80.90000000000000568, -33.89606250001229171, 102.5980762113533018 ) ) ;
#3633 = CARTESIAN_POINT ( 'NONE',  ( -82.40000000000000568, -33.43124999877096570, 102.9999999999999858 ) ) ;
#3634 = DIRECTION ( 'NONE',  ( -0.000000000000000000, -1.000000000000000000, -0.000000000000000000 ) ) ;
#3635 = AXIS2_PLACEMENT_3D ( 'NONE', #7880, #7786, #3191 ) ;
#3636 = EDGE_CURVE ( 'NONE', #7020, #15108, #7919, .T. ) ;
#3637 = CARTESIAN_POINT ( 'NONE',  ( 85.15643035625001289, -34.30312499938548854, -99.99999999999998579 ) ) ;
#3638 = CARTESIAN_POINT ( 'NONE',  ( -82.39999999999999147, -33.65624999877097423, 97.00000000000000000 ) ) ;
#3639 = CARTESIAN_POINT ( 'NONE',  ( -85.15643035625001289, -34.19062499938548427, 99.99999999999998579 ) ) ;
#3640 = CARTESIAN_POINT ( 'NONE',  ( 81.02178482187500208, -34.49062499938548854, -102.3871387122750889 ) ) ;
#3641 = ORIENTED_EDGE ( 'NONE', *, *, #5907, .T. ) ;
#3642 = CARTESIAN_POINT ( 'NONE',  ( 229.5999999999999375, -34.46249999999999147, -48.26794919243123161 ) ) ;
#3643 = CARTESIAN_POINT ( 'NONE',  ( -80.90000000000000568, -33.45000000000000284, 102.5980762113533018 ) ) ;
#3644 = CARTESIAN_POINT ( 'NONE',  ( 4.086262841041386373, 2.102637316508698451, -3.499999999999999556 ) ) ;
#3645 = CARTESIAN_POINT ( 'NONE',  ( 83.20384757729335945, -33.45134618820330985, -102.9999999999999858 ) ) ;
#3646 = FACE_OUTER_BOUND ( 'NONE', #16921, .T. ) ;
#3647 = CARTESIAN_POINT ( 'NONE',  ( -81.02178482187500208, -31.30312499938548498, 97.61286128772489690 ) ) ;
#3648 = CARTESIAN_POINT ( 'NONE',  ( 235.3564303562499447, -32.69062499938547717, -51.59142580818350865 ) ) ;
#3649 = AXIS2_PLACEMENT_3D ( 'NONE', #2665, #10746, #15244 ) ;
#3650 = CARTESIAN_POINT ( 'NONE',  ( -82.39999999999999147, -32.81250000000000000, 96.53589838486223584 ) ) ;
#3651 = ORIENTED_EDGE ( 'NONE', *, *, #770, .F. ) ;
#3652 = CARTESIAN_POINT ( 'NONE',  ( -82.39999999999999147, -33.43124999877097281, -96.99999999999998579 ) ) ;
#3653 = CARTESIAN_POINT ( 'NONE',  ( 235.5999999999999943, -33.78750000000000142, -51.73205080756900287 ) ) ;
#3654 = CARTESIAN_POINT ( 'NONE',  ( 85.15643035624999868, -33.25312499938548427, 98.40857419181659793 ) ) ;
#3655 = VECTOR ( 'NONE', #13536, 1000.000000000000000 ) ;
#3656 = CARTESIAN_POINT ( 'NONE',  ( -99.99999999999998579, -29.80000000000000426, 150.0000000000000000 ) ) ;
#3657 = CARTESIAN_POINT ( 'NONE',  ( -85.15643035625001289, -32.95312499938548711, 99.99999999999998579 ) ) ;
#3658 = VECTOR ( 'NONE', #12966, 1000.000000000000000 ) ;
#3659 = CARTESIAN_POINT ( 'NONE',  ( -82.39999999999999147, -32.84062499938548996, -96.81714838363319586 ) ) ;
#3660 = CARTESIAN_POINT ( 'NONE',  ( 79.64356964375001269, -32.20312499938548001, 98.40857419181659793 ) ) ;
#3661 = CARTESIAN_POINT ( 'NONE',  ( 82.39999999999999147, -32.39062499938548001, -103.1828516163667899 ) ) ;
#3662 = EDGE_CURVE ( 'NONE', #800, #12300, #15738, .T. ) ;
#3663 = CARTESIAN_POINT ( 'NONE',  ( 232.5999999999999375, -32.05312499938548143, -53.18285161636690361 ) ) ;
#3664 = CARTESIAN_POINT ( 'NONE',  ( -82.39999999999999147, -33.29062499938548569, 103.1828516163667899 ) ) ;
#3665 = CARTESIAN_POINT ( 'NONE',  ( -85.15643035624999868, -33.44062499938548427, -101.5914258081833879 ) ) ;
#3666 = ORIENTED_EDGE ( 'NONE', *, *, #6947, .T. ) ;
#3667 = CARTESIAN_POINT ( 'NONE',  ( 85.15643035624999868, -32.46562499938548996, 98.40857419181659793 ) ) ;
#3668 = VECTOR ( 'NONE', #5983, 1000.000000000000000 ) ;
#3669 = CARTESIAN_POINT ( 'NONE',  ( 110.9999999999999574, -21.80000000000003268, -142.6499999999999773 ) ) ;
#3670 = CARTESIAN_POINT ( 'NONE',  ( -79.64356964375001269, -31.22812499938548925, 98.40857419181659793 ) ) ;
#3671 = CARTESIAN_POINT ( 'NONE',  ( -81.02178482187500208, -35.05312499938548854, 102.3871387122750889 ) ) ;
#3672 = CARTESIAN_POINT ( 'NONE',  ( -85.40000000000000568, -31.31250000000000000, 101.7320508075688821 ) ) ;
#3673 = ORIENTED_EDGE ( 'NONE', *, *, #4882, .T. ) ;
#3674 = CARTESIAN_POINT ( 'NONE',  ( -79.39999999999999147, -32.88750000000000284, -101.7320508075688821 ) ) ;
#3675 = VECTOR ( 'NONE', #12368, 999.9999999999998863 ) ;
#3676 =( GEOMETRIC_REPRESENTATION_CONTEXT ( 3 ) GLOBAL_UNCERTAINTY_ASSIGNED_CONTEXT ( ( #15446 ) ) GLOBAL_UNIT_ASSIGNED_CONTEXT ( ( #7533, #12318, #3228 ) ) REPRESENTATION_CONTEXT ( 'NONE', 'WORKASPACE' ) );
#3677 = DIRECTION ( 'NONE',  ( 0.000000000000000000, 0.000000000000000000, -1.000000000000000000 ) ) ;
#3678 = CARTESIAN_POINT ( 'NONE',  ( 231.9572389284484757, -35.00000000000000000, -52.93757093704014949 ) ) ;
#3679 = CARTESIAN_POINT ( 'NONE',  ( -81.59615242270665192, -32.77634618820330559, 97.00000000000000000 ) ) ;
#3680 = CARTESIAN_POINT ( 'NONE',  ( 232.5999999999999375, -32.05312499938548143, 96.81714838363319586 ) ) ;
#3681 = CARTESIAN_POINT ( 'NONE',  ( -80.90000000000000568, -33.69768749875867542, 97.40192378864668399 ) ) ;
#3682 = VECTOR ( 'NONE', #15107, 1000.000000000000000 ) ;
#3683 = CARTESIAN_POINT ( 'NONE',  ( 231.7961524227065979, -32.79240381056765585, 97.00000000000000000 ) ) ;
#3684 = CARTESIAN_POINT ( 'NONE',  ( -82.40000000000001990, -32.75624999877096855, -103.0000000000000000 ) ) ;
#3685 = CARTESIAN_POINT ( 'NONE',  ( -94.79999999999999716, -35.00000000000000000, -150.0000000000000000 ) ) ;
#3686 = CARTESIAN_POINT ( 'NONE',  ( -82.40000000000000568, -30.00000000000000355, 99.99999999999998579 ) ) ;
#3687 = CARTESIAN_POINT ( 'NONE',  ( 81.02178482187500208, -30.85312499938548569, -97.61286128772489690 ) ) ;
#3688 = DIRECTION ( 'NONE',  ( 0.000000000000000000, 0.000000000000000000, 1.000000000000000000 ) ) ;
#3689 = VECTOR ( 'NONE', #15560, 1000.000000000000000 ) ;
#3690 = VERTEX_POINT ( 'NONE', #17104 ) ;
#3691 = CARTESIAN_POINT ( 'NONE',  ( 235.3564303562499447, -34.97812499938547859, -50.00000000000011369 ) ) ;
#3692 = CARTESIAN_POINT ( 'NONE',  ( 233.9782151781249411, -33.10312499938547859, 97.61286128772489690 ) ) ;
#3693 = CARTESIAN_POINT ( 'NONE',  ( 235.3564303562499447, -34.11562499938548143, -48.40857419181671162 ) ) ;
#3694 = CARTESIAN_POINT ( 'NONE',  ( -85.15643035624999868, -33.32812499938548001, 98.40857419181659793 ) ) ;
#3695 = VERTEX_POINT ( 'NONE', #6945 ) ;
#3696 = ORIENTED_EDGE ( 'NONE', *, *, #7022, .F. ) ;
#3697 = CARTESIAN_POINT ( 'NONE',  ( -81.02178482187500208, -31.19062499938548427, -102.3871387122750889 ) ) ;
#3698 = FACE_OUTER_BOUND ( 'NONE', #3723, .T. ) ;
#3699 = ORIENTED_EDGE ( 'NONE', *, *, #13345, .F. ) ;
#3700 = CARTESIAN_POINT ( 'NONE',  ( 83.77821517812500929, -33.47812499938548569, 102.3871387122750889 ) ) ;
#3701 = CARTESIAN_POINT ( 'NONE',  ( -80.90000000000000568, -33.69374999877096855, -102.5980762113533018 ) ) ;
#3702 = AXIS2_PLACEMENT_3D ( 'NONE', #4457, #16477, #12071 ) ;
#3703 = CARTESIAN_POINT ( 'NONE',  ( 82.39999999999999147, -34.61250000000000426, 103.4641016151377499 ) ) ;
#3704 = CARTESIAN_POINT ( 'NONE',  ( -80.90000000000000568, -34.35000000000000853, 102.5980762113533018 ) ) ;
#3705 = CARTESIAN_POINT ( 'NONE',  ( -79.39999999999999147, -32.41874999877096997, 99.99999999999998579 ) ) ;
#3706 = CARTESIAN_POINT ( 'NONE',  ( -85.40000000000000568, -34.48124999877096997, 98.26794919243111792 ) ) ;
#3707 = CARTESIAN_POINT ( 'NONE',  ( 85.32499745258125756, -35.00000000000000711, -99.84129707245892860 ) ) ;
#3708 = CARTESIAN_POINT ( 'NONE',  ( 231.9572389284484757, -35.00000000000000000, 97.06242906295996420 ) ) ;
#3709 = CARTESIAN_POINT ( 'NONE',  ( 82.40000000000000568, -30.00000000000000355, 96.99999999999998579 ) ) ;
#3710 = CARTESIAN_POINT ( 'NONE',  ( 233.9782151781249411, -33.59062499938547575, 102.3871387122750889 ) ) ;
#3711 = EDGE_LOOP ( 'NONE', ( #3889, #17571, #13602, #7033 ) ) ;
#3712 = CARTESIAN_POINT ( 'NONE',  ( 82.39999999999999147, -32.95312499938548711, -96.81714838363319586 ) ) ;
#3713 = PRESENTATION_STYLE_ASSIGNMENT (( #17102 ) ) ;
#3714 = CARTESIAN_POINT ( 'NONE',  ( 232.5999999999999375, -31.40624999877096712, 96.53589838486223584 ) ) ;
#3715 = CARTESIAN_POINT ( 'NONE',  ( 234.0999999999999375, -31.44374999877096144, -52.59807621135342970 ) ) ;
#3716 = ORIENTED_EDGE ( 'NONE', *, *, #9335, .F. ) ;
#3717 = DIRECTION ( 'NONE',  ( 0.000000000000000000, 1.000000000000000000, 0.000000000000000000 ) ) ;
#3718 = CARTESIAN_POINT ( 'NONE',  ( -82.40000000000000568, -30.00000000000000355, 99.99999999999998579 ) ) ;
#3719 = CARTESIAN_POINT ( 'NONE',  ( 244.7999999999999545, -29.80000000000003268, -103.0000000000000284 ) ) ;
#3720 = ORIENTED_EDGE ( 'NONE', *, *, #14601, .F. ) ;
#3721 = CARTESIAN_POINT ( 'NONE',  ( -85.40000000000000568, -33.99374999877097281, -99.99999999999998579 ) ) ;
#3722 = CARTESIAN_POINT ( 'NONE',  ( 4.124214193018032049, -2.028338413290972753, 3.513185186763607248 ) ) ;
#3723 = EDGE_LOOP ( 'NONE', ( #3194, #2426, #5492, #8499 ) ) ;
#3724 = FILL_AREA_STYLE ('',( #15844 ) ) ;
#3725 = CARTESIAN_POINT ( 'NONE',  ( 85.40000000000000568, -30.93750000000000355, -98.26794919243111792 ) ) ;
#3726 = CARTESIAN_POINT ( 'NONE',  ( -83.90000000000000568, -30.46874999877096712, 97.40192378864668399 ) ) ;
#3727 = CARTESIAN_POINT ( 'NONE',  ( -85.40000000000000568, -34.89374999877097139, 99.99999999999998579 ) ) ;
#3728 = CARTESIAN_POINT ( 'NONE',  ( -82.39999999999999147, -30.56250000000000355, 96.53589838486223584 ) ) ;
#3729 = CARTESIAN_POINT ( 'NONE',  ( 232.5880334581522106, -34.99999999999999289, -52.99916460278299013 ) ) ;
#3730 = CARTESIAN_POINT ( 'NONE',  ( 230.4884518427504076, -35.14114861271050216, 98.22820072003833047 ) ) ;
#3731 = CARTESIAN_POINT ( 'NONE',  ( 85.15643035625001289, -34.71562499938548285, -101.5914258081833879 ) ) ;
#3732 = DIRECTION ( 'NONE',  ( 0.000000000000000000, 0.000000000000000000, 1.000000000000000000 ) ) ;
#3733 = CARTESIAN_POINT ( 'NONE',  ( -79.64356964375001269, -34.37812499938548427, 98.40857419181659793 ) ) ;
#3734 = CARTESIAN_POINT ( 'NONE',  ( -82.39999999999999147, -31.01249999999999929, 96.99999999999998579 ) ) ;
#3735 = ORIENTED_EDGE ( 'NONE', *, *, #10245, .T. ) ;
#3736 = CARTESIAN_POINT ( 'NONE',  ( 82.39999999999999147, -32.81250000000000000, 103.0000000000000000 ) ) ;
#3737 = CARTESIAN_POINT ( 'NONE',  ( -85.40000000000000568, -34.01250000000000284, 101.7320508075688679 ) ) ;
#3738 = CARTESIAN_POINT ( 'NONE',  ( -0.5276280594146446346, 4.314175951381965746, -3.320322319201721495 ) ) ;
#3739 = CARTESIAN_POINT ( 'NONE',  ( 82.39999999999999147, -33.48750000000000426, 97.00000000000000000 ) ) ;
#3740 = CARTESIAN_POINT ( 'NONE',  ( -79.64356964375001269, -33.14062499938548711, 98.40857419181659793 ) ) ;
#3741 = CARTESIAN_POINT ( 'NONE',  ( 231.2217848218749339, -34.82812499938548001, -52.38713871227520968 ) ) ;
#3742 = ADVANCED_FACE ( 'NONE', ( #3806 ), #5585, .F. ) ;
#3743 = EDGE_LOOP ( 'NONE', ( #11940, #1148, #11091, #1297 ) ) ;
#3744 = CARTESIAN_POINT ( 'NONE',  ( 4.030875481281934292, 1.403567514398448068, 3.500000000000000000 ) ) ;
#3745 = CARTESIAN_POINT ( 'NONE',  ( 80.17984880387892588, -34.99999999999998579, 98.35655086105387568 ) ) ;
#3746 = CARTESIAN_POINT ( 'NONE',  ( 85.15643035624999868, -32.87812499938549138, 101.5914258081833879 ) ) ;
#3747 = CARTESIAN_POINT ( 'NONE',  ( -4.000000000000000000, 0.000000000000000000, 0.000000000000000000 ) ) ;
#3748 = CARTESIAN_POINT ( 'NONE',  ( 232.5999999999999943, -32.95312499938548001, -53.18285161636690361 ) ) ;
#3749 = ADVANCED_FACE ( 'NONE', ( #18866 ), #6035, .F. ) ;
#3750 = CARTESIAN_POINT ( 'NONE',  ( -83.77821517812500929, -34.82812499938548711, 97.61286128772489690 ) ) ;
#3751 = CARTESIAN_POINT ( 'NONE',  ( 4.175813232069147674, 2.061359961916367833, 3.570380186727398097 ) ) ;
#3752 = CARTESIAN_POINT ( 'NONE',  ( 83.77821517812500929, -32.46562499938548285, 102.3871387122750889 ) ) ;
#3753 = EDGE_CURVE ( 'NONE', #13349, #7832, #678, .T. ) ;
#3754 = CARTESIAN_POINT ( 'NONE',  ( 85.15643035625001289, -30.14062499938548711, -99.99999999999998579 ) ) ;
#3755 = CARTESIAN_POINT ( 'NONE',  ( 229.8435696437499871, -33.70312499938548001, -48.40857419181671162 ) ) ;
#3756 = CARTESIAN_POINT ( 'NONE',  ( -85.15643035625001289, -34.75312499938548427, 99.99999999999998579 ) ) ;
#3757 = CARTESIAN_POINT ( 'NONE',  ( -82.39999999999999147, -31.82812499938548356, -96.81714838363319586 ) ) ;
#3758 = ADVANCED_FACE ( 'NONE', ( #1542 ), #14618, .T. ) ;
#3759 = ORIENTED_EDGE ( 'NONE', *, *, #3769, .F. ) ;
#3760 = CARTESIAN_POINT ( 'NONE',  ( 85.15643035624999868, -32.01562499938548711, 98.40857419181659793 ) ) ;
#3761 = CARTESIAN_POINT ( 'NONE',  ( 234.0999999999999375, -32.79374999877096286, 97.40192378864668399 ) ) ;
#3762 = CARTESIAN_POINT ( 'NONE',  ( -85.40000000000000568, -33.63750000000000284, 98.26794919243111792 ) ) ;
#3763 = CARTESIAN_POINT ( 'NONE',  ( -85.15643035624999868, -31.07812499938548356, 98.40857419181659793 ) ) ;
#3764 = CARTESIAN_POINT ( 'NONE',  ( -85.15643035625001289, -34.75312499938548427, 99.99999999999998579 ) ) ;
#3765 = CARTESIAN_POINT ( 'NONE',  ( 84.70388354820681798, -35.00002705695767702, 101.9214814096700934 ) ) ;
#3766 = VERTEX_POINT ( 'NONE', #17660 ) ;
#3767 = CARTESIAN_POINT ( 'NONE',  ( -85.40000000000000568, -33.14999999999999858, -99.99999999999998579 ) ) ;
#3768 = CARTESIAN_POINT ( 'NONE',  ( -81.59615242270660929, -32.32634618820329564, 96.99999999999997158 ) ) ;
#3769 = EDGE_CURVE ( 'NONE', #8657, #13128, #11883, .T. ) ;
#3770 = CARTESIAN_POINT ( 'NONE',  ( -79.39999999999999147, -30.63356250001229242, 98.26794919243110371 ) ) ;
#3771 = CARTESIAN_POINT ( 'NONE',  ( -82.39999999999999147, -34.11018749875866973, 96.53589838486223584 ) ) ;
#3772 = CARTESIAN_POINT ( 'NONE',  ( -83.04276107155152431, -35.00000000000000000, 97.06242906295996420 ) ) ;
#3773 = CARTESIAN_POINT ( 'NONE',  ( -79.39999999999999147, -33.28124999877096712, -101.7320508075688963 ) ) ;
#3774 = CARTESIAN_POINT ( 'NONE',  ( 230.0666556977843982, -31.99999999999997868, 101.1009827666099596 ) ) ;
#3775 = FACE_OUTER_BOUND ( 'NONE', #4438, .T. ) ;
#3776 = DIRECTION ( 'NONE',  ( 0.000000000000000000, 0.000000000000000000, 1.000000000000000000 ) ) ;
#3777 = CARTESIAN_POINT ( 'NONE',  ( 110.0000000000000000, 5.199999999999952216, 50.00000000000001421 ) ) ;
#3778 = CARTESIAN_POINT ( 'NONE',  ( 83.77821517812500929, -30.77812499938548640, -97.61286128772489690 ) ) ;
#3779 = CARTESIAN_POINT ( 'NONE',  ( 4.175075985190095373, 2.060370777630105898, 3.568666869285574972 ) ) ;
#3780 = VERTEX_POINT ( 'NONE', #16199 ) ;
#3781 = DIRECTION ( 'NONE',  ( -2.775557561562891351E-15, -1.000000000000000000, 0.000000000000000000 ) ) ;
#3782 = APPLICATION_PROTOCOL_DEFINITION ( 'draft international standard', 'automotive_design', 1998, #4709 ) ;
#3783 = CARTESIAN_POINT ( 'NONE',  ( 232.5999999999999375, -32.16562499938547859, 96.81714838363319586 ) ) ;
#3784 = EDGE_CURVE ( 'NONE', #15956, #12903, #8032, .T. ) ;
#3785 = CARTESIAN_POINT ( 'NONE',  ( 235.3564303562499447, -33.59062499938548285, -51.59142580818350865 ) ) ;
#3786 = CARTESIAN_POINT ( 'NONE',  ( -85.15643035625001289, -34.19062499938548427, 99.99999999999998579 ) ) ;
#3787 = CARTESIAN_POINT ( 'NONE',  ( 85.40000000000000568, -34.05000000000000426, 99.99999999999998579 ) ) ;
#3788 = VERTEX_POINT ( 'NONE', #4177 ) ;
#3789 = CARTESIAN_POINT ( 'NONE',  ( -83.77821517812500929, -32.76562499938548711, -97.61286128772489690 ) ) ;
#3790 = CARTESIAN_POINT ( 'NONE',  ( -85.15643035625001289, -30.14062499938548711, 99.99999999999998579 ) ) ;
#3791 = ORIENTED_EDGE ( 'NONE', *, *, #4723, .T. ) ;
#3792 = CARTESIAN_POINT ( 'NONE',  ( 82.39999999999999147, -33.51562499938548711, 103.1828516163667899 ) ) ;
#3793 = CARTESIAN_POINT ( 'NONE',  ( -83.90000000000000568, -33.61874999877097281, -102.5980762113533018 ) ) ;
#3794 = CARTESIAN_POINT ( 'NONE',  ( 79.39999999999999147, -34.68750000000000000, 101.7320508075688821 ) ) ;
#3795 = CARTESIAN_POINT ( 'NONE',  ( 25.60000000000000142, 0.000000000000000000, 0.000000000000000000 ) ) ;
#3796 = CARTESIAN_POINT ( 'NONE',  ( -82.39999999999999147, -32.53124999877096712, 103.4641016151377499 ) ) ;
#3797 = CARTESIAN_POINT ( 'NONE',  ( -85.15643035625001289, -30.70312499938548711, 99.99999999999998579 ) ) ;
#3798 = CARTESIAN_POINT ( 'NONE',  ( -83.77821517812500929, -32.31562499938548427, -97.61286128772489690 ) ) ;
#3799 = VECTOR ( 'NONE', #3422, 1000.000000000000000 ) ;
#3800 = CARTESIAN_POINT ( 'NONE',  ( 96.99999999999997158, -5.200000000000003730, -150.0000000000000000 ) ) ;
#3801 = CARTESIAN_POINT ( 'NONE',  ( 234.7546687845694180, -31.99999999999997868, 102.0417045141626176 ) ) ;
#3802 = CARTESIAN_POINT ( 'NONE',  ( 233.9782151781249411, -32.99062499938548143, 97.61286128772489690 ) ) ;
#3803 = ORIENTED_EDGE ( 'NONE', *, *, #3099, .T. ) ;
#3804 = CARTESIAN_POINT ( 'NONE',  ( 83.77821517812500929, -32.31562499938548427, -102.3871387122750889 ) ) ;
#3805 = CARTESIAN_POINT ( 'NONE',  ( -82.39999999999999147, -34.97812499938547859, -96.81714838363319586 ) ) ;
#3806 = FACE_OUTER_BOUND ( 'NONE', #2608, .T. ) ;
#3807 = EDGE_LOOP ( 'NONE', ( #13200, #12509, #16817, #5093, #368, #10022 ) ) ;
#3808 = CARTESIAN_POINT ( 'NONE',  ( 231.0999999999999375, -32.56874999877096144, 102.5980762113533018 ) ) ;
#3809 = CARTESIAN_POINT ( 'NONE',  ( -81.02178482187500208, -30.44062499938548783, 102.3871387122750889 ) ) ;
#3810 = CARTESIAN_POINT ( 'NONE',  ( 81.59615242270663771, -32.11740381056766580, 96.99999999999998579 ) ) ;
#3811 = ORIENTED_EDGE ( 'NONE', *, *, #8428, .T. ) ;
#3812 = CARTESIAN_POINT ( 'NONE',  ( 3.974175853610053100, -3.450041667725632699, 1.156004144284124457 ) ) ;
#3813 = VECTOR ( 'NONE', #5408, 1000.000000000000000 ) ;
#3814 = AXIS2_PLACEMENT_3D ( 'NONE', #11860, #1415, #9118 ) ;
#3815 = CARTESIAN_POINT ( 'NONE',  ( 234.0999999999999375, -33.69374999877096144, -52.59807621135342970 ) ) ;
#3816 = ORIENTED_EDGE ( 'NONE', *, *, #11616, .F. ) ;
#3817 = CARTESIAN_POINT ( 'NONE',  ( 85.40000000000000568, -33.63750000000000284, -98.26794919243111792 ) ) ;
#3818 = FACE_OUTER_BOUND ( 'NONE', #13329, .T. ) ;
#3819 = CARTESIAN_POINT ( 'NONE',  ( -85.15643035625001289, -32.05312499938548854, 99.99999999999998579 ) ) ;
#3820 = CARTESIAN_POINT ( 'NONE',  ( -85.40000000000000568, -29.97835047384105067, 100.9999487804559664 ) ) ;
#3821 = CARTESIAN_POINT ( 'NONE',  ( -69.99999999999998579, -35.00000000000000000, -150.0000000000000000 ) ) ;
#3822 = CARTESIAN_POINT ( 'NONE',  ( 231.0999999999999375, -33.22499999999999432, 97.40192378864668399 ) ) ;
#3823 = CARTESIAN_POINT ( 'NONE',  ( 83.90000000000000568, -33.91874999877096997, 97.40192378864668399 ) ) ;
#3824 = CARTESIAN_POINT ( 'NONE',  ( 80.90000000000000568, -33.89999999999999858, 97.40192378864668399 ) ) ;
#3825 = CARTESIAN_POINT ( 'NONE',  ( -82.39999999999999147, -32.50312499938548427, 96.81714838363319586 ) ) ;
#3826 = CIRCLE ( 'NONE', #1961, 3.500000000000000000 ) ;
#3827 = CONICAL_SURFACE ( 'NONE', #8824, 5.560781378645573980, 1.221730476396046816 ) ;
#3828 = DIRECTION ( 'NONE',  ( 0.000000000000000000, 0.000000000000000000, 1.000000000000000000 ) ) ;
#3829 = ORIENTED_EDGE ( 'NONE', *, *, #12104, .T. ) ;
#3830 = CARTESIAN_POINT ( 'NONE',  ( 79.39999999999999147, -32.88750000000000284, 101.7320508075688963 ) ) ;
#3831 = DIRECTION ( 'NONE',  ( -0.000000000000000000, -1.000000000000000000, -0.000000000000000000 ) ) ;
#3832 = CARTESIAN_POINT ( 'NONE',  ( -2.807080416178626692, 3.225969019225154444, -3.502507215260441065 ) ) ;
#3833 = CARTESIAN_POINT ( 'NONE',  ( 233.9782151781249411, -34.90312499938547575, 97.61286128772489690 ) ) ;
#3834 = CARTESIAN_POINT ( 'NONE',  ( -82.39999999999999147, -33.29062499938549280, 103.1828516163667899 ) ) ;
#3835 = CARTESIAN_POINT ( 'NONE',  ( 233.9782151781249411, -30.74062499938547788, -52.38713871227520968 ) ) ;
#3836 = ORIENTED_EDGE ( 'NONE', *, *, #16768, .T. ) ;
#3837 =( REPRESENTATION_RELATIONSHIP ('NONE','NONE', #14468, #7631 ) REPRESENTATION_RELATIONSHIP_WITH_TRANSFORMATION ( #5837 )SHAPE_REPRESENTATION_RELATIONSHIP( ) );
#3838 = CARTESIAN_POINT ( 'NONE',  ( -80.98256025945210013, -35.00066800082266383, 97.35069876254466692 ) ) ;
#3839 = CARTESIAN_POINT ( 'NONE',  ( -85.15643035624999868, -35.05312499938548143, 101.5914258081833879 ) ) ;
#3840 = AXIS2_PLACEMENT_3D ( 'NONE', #9295, #16725, #12138 ) ;
#3841 = CARTESIAN_POINT ( 'NONE',  ( -84.70833260042415702, -35.00006955123599539, 98.08383195543535749 ) ) ;
#3842 = CARTESIAN_POINT ( 'NONE',  ( 85.15643035625001289, -33.29062499938547859, 99.99999999999998579 ) ) ;
#3843 = CARTESIAN_POINT ( 'NONE',  ( -3.540020015735593439, -2.810662092924100630, -3.602146406945814672 ) ) ;
#3844 = ADVANCED_FACE ( 'NONE', ( #1151 ), #13149, .T. ) ;
#3845 = CARTESIAN_POINT ( 'NONE',  ( 82.40000000000001990, -32.75624999877096855, -97.00000000000000000 ) ) ;
#3846 = CARTESIAN_POINT ( 'NONE',  ( -85.15643035625001289, -34.34062499938548285, 98.40857419181659793 ) ) ;
#3847 = CARTESIAN_POINT ( 'NONE',  ( -85.15643035625001289, -34.34062499938548285, -101.5914258081833879 ) ) ;
#3848 = CARTESIAN_POINT ( 'NONE',  ( 82.39999999999999147, -31.15312499938548640, 103.1828516163667899 ) ) ;
#3849 = ADVANCED_FACE ( 'NONE', ( #4272 ), #16288, .F. ) ;
#3850 = B_SPLINE_CURVE_WITH_KNOTS ( 'NONE', 3,
 ( #13565, #15425, #492, #9171, #16606, #18367, #18081, #9460, #9074, #7517, #4592, #10550, #1661, #1750, #3308, #206 ),
 .UNSPECIFIED., .F., .F.,
 ( 4, 3, 3, 3, 3, 4 ),
 ( -2.111273352580990396E-06, 0.000000000000000000, 3.519286887793134604E-05, 7.191842652045515611E-05, 0.0001049868727088832553, 0.0001382836236814611892 ),
 .UNSPECIFIED. ) ;
#3851 = EDGE_CURVE ( 'NONE', #10258, #15900, #8532, .T. ) ;
#3852 = CARTESIAN_POINT ( 'NONE',  ( 83.77821517812500929, -33.77812499938548285, -102.3871387122750889 ) ) ;
#3853 = CARTESIAN_POINT ( 'NONE',  ( 231.2217848218749339, -33.81562499938547717, -52.38713871227520968 ) ) ;
#3854 = CARTESIAN_POINT ( 'NONE',  ( -79.64356964374998427, -32.20312499938548711, 101.5914258081833879 ) ) ;
#3855 = CARTESIAN_POINT ( 'NONE',  ( 79.64356964375001269, -30.77812499938548285, -98.40857419181659793 ) ) ;
#3856 = ORIENTED_EDGE ( 'NONE', *, *, #12684, .T. ) ;
#3857 = CARTESIAN_POINT ( 'NONE',  ( 83.77821517812500929, -32.87812499938548427, 97.61286128772489690 ) ) ;
#3858 = CARTESIAN_POINT ( 'NONE',  ( -0.1750025118121544265, -4.719839900820635314, -3.469254087858253399 ) ) ;
#3859 = B_SPLINE_CURVE_WITH_KNOTS ( 'NONE', 3,
 ( #2044, #18466, #8003, #11520, #7122, #16109, #14245, #3893, #11325, #6742, #11226, #2615, #12885, #5281, #15915, #18758, #14531, #12689 ),
 .UNSPECIFIED., .F., .F.,
 ( 4, 2, 2, 2, 2, 2, 2, 2, 4 ),
 ( 0.000000000000000000, 0.0007106627595358718397, 0.001421325519071743679, 0.002131988278607615736, 0.002842651038143487359, 0.003553313797679358982, 0.004263976557215231472, 0.004974639316751103095, 0.005685302076286974718 ),
 .UNSPECIFIED. ) ;
#3860 = CARTESIAN_POINT ( 'NONE',  ( -82.39999999999999147, -33.26250000000000284, 96.53589838486223584 ) ) ;
#3861 = CARTESIAN_POINT ( 'NONE',  ( -82.39999999999999147, -30.25312499938548783, 96.81714838363319586 ) ) ;
#3862 = CARTESIAN_POINT ( 'NONE',  ( -83.77821517812500929, -30.96562499938548640, 102.3871387122750889 ) ) ;
#3863 = CARTESIAN_POINT ( 'NONE',  ( 4.630153689607048761, 0.000000000000000000, 0.000000000000000000 ) ) ;
#3864 = ORIENTED_EDGE ( 'NONE', *, *, #6640, .T. ) ;
#3865 = CARTESIAN_POINT ( 'NONE',  ( -80.90000000000000568, -33.45000000000000284, -97.40192378864668399 ) ) ;
#3866 = ADVANCED_FACE ( 'NONE', ( #3646 ), #17133, .F. ) ;
#3867 = CARTESIAN_POINT ( 'NONE',  ( 1.393927851585479161, -4.043713361053543842, -3.526374918436840922 ) ) ;
#3868 = CARTESIAN_POINT ( 'NONE',  ( -82.40000000000000568, -30.00000000000000355, 96.99999999999998579 ) ) ;
#3869 = DIRECTION ( 'NONE',  ( 1.387778780781445676E-15, 1.000000000000000000, -2.775557561562891351E-15 ) ) ;
#3870 = EDGE_CURVE ( 'NONE', #4219, #10782, #7908, .T. ) ;
#3871 = CARTESIAN_POINT ( 'NONE',  ( -81.59615242270662350, -34.63259618943234130, 96.99999999999997158 ) ) ;
#3872 = CARTESIAN_POINT ( 'NONE',  ( -83.60689295392862164, -35.00000000000000000, 97.24646917567288540 ) ) ;
#3873 = CARTESIAN_POINT ( 'NONE',  ( -79.64356964374999848, -30.36562499938548498, 99.99999999999998579 ) ) ;
#3874 = CARTESIAN_POINT ( 'NONE',  ( 2.100000000000000089, 0.000000000000000000, -4.694516984716113228 ) ) ;
#3875 = CARTESIAN_POINT ( 'NONE',  ( 4.630153689607048761, 0.000000000000000000, 0.000000000000000000 ) ) ;
#3876 = CARTESIAN_POINT ( 'NONE',  ( 110.0000000000000000, 5.199999999999975309, -145.0000000000000000 ) ) ;
#3877 = DIRECTION ( 'NONE',  ( 0.000000000000000000, -1.000000000000000000, 0.000000000000000000 ) ) ;
#3878 = CARTESIAN_POINT ( 'NONE',  ( 85.15643035624999868, -34.71562499938548285, -101.5914258081833879 ) ) ;
#3879 = CARTESIAN_POINT ( 'NONE',  ( -83.20384757729335945, -33.00134618820329990, 102.9999999999999858 ) ) ;
#3880 = EDGE_LOOP ( 'NONE', ( #7043, #429, #14545, #8264 ) ) ;
#3881 = CARTESIAN_POINT ( 'NONE',  ( 85.40000000000000568, -30.84374999877096712, 99.99999999999998579 ) ) ;
#3882 = CONTEXT_DEPENDENT_SHAPE_REPRESENTATION ( #15578, #14188 ) ;
#3883 = CARTESIAN_POINT ( 'NONE',  ( 232.5002178375173116, -35.00000000000000711, -47.23961338448017955 ) ) ;
#3884 = CARTESIAN_POINT ( 'NONE',  ( 233.9782151781249411, -32.65312499938548285, -52.38713871227520968 ) ) ;
#3885 = CARTESIAN_POINT ( 'NONE',  ( -83.77821517812500929, -35.01562499938548711, 102.3871387122750889 ) ) ;
#3886 = ORIENTED_EDGE ( 'NONE', *, *, #5074, .T. ) ;
#3887 = CARTESIAN_POINT ( 'NONE',  ( -82.39999999999999147, -30.70312499938548711, -103.1828516163667899 ) ) ;
#3888 = LINE ( 'NONE', #8570, #14101 ) ;
#3889 = ORIENTED_EDGE ( 'NONE', *, *, #9772, .F. ) ;
#3890 = CARTESIAN_POINT ( 'NONE',  ( 81.02178482187500208, -33.25312499938548427, 97.61286128772489690 ) ) ;
#3891 = CARTESIAN_POINT ( 'NONE',  ( -79.64356964375001269, -31.86562499938548143, -98.40857419181659793 ) ) ;
#3892 = CARTESIAN_POINT ( 'NONE',  ( 79.39999999999999147, -33.41250000000000142, 98.26794919243113213 ) ) ;
#3893 = CARTESIAN_POINT ( 'NONE',  ( -80.48808202378405952, -34.99999999999999289, 97.80480077079599255 ) ) ;
#3894 = CARTESIAN_POINT ( 'NONE',  ( -83.90000000000000568, -34.51874999877097139, 97.40192378864668399 ) ) ;
#3895 = B_SPLINE_CURVE_WITH_KNOTS ( 'NONE', 3,
 ( #16154, #7066, #18802, #10100, #12927, #8722, #6886, #5706, #4137, #4044 ),
 .UNSPECIFIED., .F., .F.,
 ( 4, 2, 2, 2, 4 ),
 ( 0.3612006186103786654, 0.3925526867148934063, 0.4239047548194081472, 0.4552568229239228881, 0.4866088910284376290 ),
 .UNSPECIFIED. ) ;
#3896 = CARTESIAN_POINT ( 'NONE',  ( -85.15643035624999868, -30.74062499938548143, 98.40857419181659793 ) ) ;
#3897 = CARTESIAN_POINT ( 'NONE',  ( -85.15643035625001289, -32.35312499938548569, -98.40857419181659793 ) ) ;
#3898 = PRODUCT_DEFINITION_SHAPE ( 'NONE', 'NONE',  #6427 ) ;
#3899 = CARTESIAN_POINT ( 'NONE',  ( 229.5999999999999375, -32.28749999999999432, -51.73205080756898866 ) ) ;
#3900 = CARTESIAN_POINT ( 'NONE',  ( -82.39999999999999147, -34.33124999877097139, 103.0000000000000000 ) ) ;
#3901 = CARTESIAN_POINT ( 'NONE',  ( 232.5999999999999375, -30.33749999999999503, 103.4641016151377499 ) ) ;
#3902 = ORIENTED_EDGE ( 'NONE', *, *, #12813, .F. ) ;
#3903 = CARTESIAN_POINT ( 'NONE',  ( 79.64356964374999848, -32.16562499938548569, -99.99999999999998579 ) ) ;
#3904 = EDGE_CURVE ( 'NONE', #10663, #1022, #8022, .T. ) ;
#3905 = CARTESIAN_POINT ( 'NONE',  ( 229.5999999999999375, -34.03124999877096002, 98.26794919243111792 ) ) ;
#3906 = CARTESIAN_POINT ( 'NONE',  ( 232.5999999999999375, -30.95624999877096428, -53.46410161513786363 ) ) ;
#3907 = VERTEX_POINT ( 'NONE', #4038 ) ;
#3908 = CARTESIAN_POINT ( 'NONE',  ( 83.90000000000000568, -32.77499999999999858, 102.5980762113533018 ) ) ;
#3909 = CARTESIAN_POINT ( 'NONE',  ( -85.15643035625001289, -31.45312499938548356, 101.5914258081833879 ) ) ;
#3910 = DIRECTION ( 'NONE',  ( 0.000000000000000000, -1.000000000000000000, 0.000000000000000000 ) ) ;
#3911 = ORIENTED_EDGE ( 'NONE', *, *, #908, .F. ) ;
#3912 = CARTESIAN_POINT ( 'NONE',  ( -82.40000000000000568, -34.10624999877096997, -102.9999999999999858 ) ) ;
#3913 = VECTOR ( 'NONE', #16703, 1000.000000000000000 ) ;
#3914 = LINE ( 'NONE', #8313, #5382 ) ;
#3915 = VERTEX_POINT ( 'NONE', #6970 ) ;
#3916 =( BOUNDED_CURVE ( )  B_SPLINE_CURVE ( 2, ( #2754, #824, #6783, #12731, #7246, #11740, #3133, #13399, #5786 ),
 .UNSPECIFIED., .F., .F. ) 
 B_SPLINE_CURVE_WITH_KNOTS ( ( 3, 2, 2, 2, 3 ),
 ( 0.5208333333333331483, 0.5277777777777777901, 0.5416666666666666297, 0.5555555555555555802, 0.5625000000000001110 ),
 .UNSPECIFIED. ) 
 CURVE ( )  GEOMETRIC_REPRESENTATION_ITEM ( )  RATIONAL_B_SPLINE_CURVE ( ( 0.9330127018922194093, 0.9330127018922177440, 1.000000000000000000, 0.8660254037844387076, 1.000000000000000000, 0.8660254037844387076, 1.000000000000000000, 0.9330127018922182991, 0.9330127018922194093 ) ) 
 REPRESENTATION_ITEM ( '' )  );
#3917 = SURFACE_SIDE_STYLE ('',( #6670 ) ) ;
#3918 = CARTESIAN_POINT ( 'NONE',  ( 85.40000000000000568, -31.83750000000000568, -98.26794919243111792 ) ) ;
#3919 = CARTESIAN_POINT ( 'NONE',  ( 111.0000000000000000, 6.932050807568743700, -150.0000000000000000 ) ) ;
#3920 = CARTESIAN_POINT ( 'NONE',  ( -81.02178482187500208, -30.55312499938548854, 102.3871387122750889 ) ) ;
#3921 = CARTESIAN_POINT ( 'NONE',  ( -83.90000000000000568, -30.82500000000000284, 102.5980762113533018 ) ) ;
#3922 = CARTESIAN_POINT ( 'NONE',  ( -80.90000000000000568, -34.64999999999999858, -102.5980762113533018 ) ) ;
#3923 = DIRECTION ( 'NONE',  ( 0.000000000000000000, 0.000000000000000000, 1.000000000000000000 ) ) ;
#3924 = CARTESIAN_POINT ( 'NONE',  ( 229.5999999999999375, -32.19374999877096144, -50.00000000000011369 ) ) ;
#3925 = EDGE_CURVE ( 'NONE', #13993, #17953, #4299, .T. ) ;
#3926 = CARTESIAN_POINT ( 'NONE',  ( -79.39999999999999147, -33.73124999877096997, 98.26794919243110371 ) ) ;
#3927 = DIRECTION ( 'NONE',  ( 0.000000000000000000, 0.000000000000000000, -1.000000000000000000 ) ) ;
#3928 = AXIS2_PLACEMENT_3D ( 'NONE', #1133, #7279, #10315 ) ;
#3929 = CARTESIAN_POINT ( 'NONE',  ( -79.39999999999999147, -31.16249999999999787, 101.7320508075688537 ) ) ;
#3930 = ORIENTED_EDGE ( 'NONE', *, *, #695, .F. ) ;
#3931 = CARTESIAN_POINT ( 'NONE',  ( 232.5999999999999375, -34.38749999999999574, -46.53589838486234953 ) ) ;
#3932 = CARTESIAN_POINT ( 'NONE',  ( 233.2908335840015184, -34.99999999999998579, 97.11314983874018480 ) ) ;
#3933 = CARTESIAN_POINT ( 'NONE',  ( -96.99999999999998579, -29.80000000000000426, -150.0000000000000000 ) ) ;
#3934 = CARTESIAN_POINT ( 'NONE',  ( 235.3564303562499447, -34.97812499938547859, 99.99999999999998579 ) ) ;
#3935 = CARTESIAN_POINT ( 'NONE',  ( -81.02178482187500208, -34.60312499938549280, 102.3871387122750889 ) ) ;
#3936 = CARTESIAN_POINT ( 'NONE',  ( 231.2217848218749339, -34.67812499938548143, -47.61286128772501769 ) ) ;
#3937 = ORIENTED_EDGE ( 'NONE', *, *, #18192, .F. ) ;
#3938 = CARTESIAN_POINT ( 'NONE',  ( 232.5999999999999659, -32.13749999999999574, -47.00000000000011369 ) ) ;
#3939 = CARTESIAN_POINT ( 'NONE',  ( -82.39999999999999147, -33.62812499938549138, 103.1828516163667899 ) ) ;
#3940 = CIRCLE ( 'NONE', #9874, 6.000000000000005329 ) ;
#3941 = FACE_OUTER_BOUND ( 'NONE', #10610, .T. ) ;
#3942 = CARTESIAN_POINT ( 'NONE',  ( 80.90000000000000568, -30.60000000000000142, 102.5980762113533018 ) ) ;
#3943 = EDGE_CURVE ( 'NONE', #17562, #9205, #7011, .T. ) ;
#3944 = LINE ( 'NONE', #1026, #17424 ) ;
#3945 = CARTESIAN_POINT ( 'NONE',  ( 231.2217848218749339, -32.01562499938548001, -52.38713871227520968 ) ) ;
#3946 =( BOUNDED_CURVE ( )  B_SPLINE_CURVE ( 2, ( #1852, #7810, #13765, #402, #8000, #7904, #4991, #16901, #15429, #2041, #18558, #17287, #3601, #14241, #6643, #14431, #12879, #6931, #14338, #1065, #18851, #17088, #14056, #784, #14150, #17379, #5173, #9759, #12590, #11418, #5374, #8103, #2233, #11120, #3890, #12975, #690, #7021, #976, #15722, #3700, #3792, #8387, #15627, #15819, #9667, #8199, #2427, #6739, #5473, #12685, #18946, #16989, #9857, #11223, #2328, #3992, #18658, #8474, #9958, #15912, #2517, #11026, #5277, #879, #8291, #17188, #6842, #12786, #9563, #15528, #18755, #11321, #2145, #14922, #14720, #2712, #19038, #1260, #4184, #2612, #16207, #17573 ),
 .UNSPECIFIED., .F., .F. ) 
 B_SPLINE_CURVE_WITH_KNOTS ( ( 3, 2, 2, 2, 2, 2, 2, 2, 2, 2, 2, 2, 2, 2, 2, 2, 2, 2, 2, 2, 2, 2, 2, 2, 2, 2, 2, 2, 2, 2, 2, 2, 2, 2, 2, 2, 2, 2, 2, 2, 2, 3 ),
 ( 0.3495698921800945436, 0.3600184345287981147, 0.3750192026341647167, 0.3900199707395312632, 0.4050207388448978651, 0.4200215069502644671, 0.4350222750556310691, 0.4500230431609976156, 0.4650238112663642176, 0.4800245793717307086, 0.4950253474770973661, 0.5100261155824639125, 0.5250268836878304590, 0.5400276517931971165, 0.5550284198985636630, 0.5700291880039303205, 0.5850299561092967560, 0.6000307242146634135, 0.6150314923200299599, 0.6300322604253966174, 0.6450330285307631639, 0.6600337966361298214, 0.6750345647414963679, 0.6900353328468629144, 0.7050361009522294609, 0.7200368690575960073, 0.7350376371629626648, 0.7500384052683293223, 0.7650391733736958688, 0.7800399414790624153, 0.7950407095844290728, 0.8100414776897955083, 0.8250422457951621658, 0.8400430139005288233, 0.8550437820058953697, 0.8700445501112619162, 0.8850453182166284627, 0.9000460863219952312, 0.9150468544273615557, 0.9300476225327283242, 0.9450483906380948707, 0.9496006163947576795 ),
 .UNSPECIFIED. ) 
 CURVE ( )  GEOMETRIC_REPRESENTATION_ITEM ( )  RATIONAL_B_SPLINE_CURVE ( ( 0.9433623850486869689, 0.9066821623815414233, 1.000000000000000000, 0.8660254037844387076, 1.000000000000000000, 0.8660254037844387076, 1.000000000000000000, 0.8660254037844387076, 1.000000000000000000, 0.8660254037844387076, 1.000000000000000000, 0.8660254037844387076, 1.000000000000000000, 0.8660254037844387076, 1.000000000000000000, 0.8660254037844387076, 1.000000000000000000, 0.8660254037844387076, 1.000000000000000000, 0.8660254037844387076, 1.000000000000000000, 0.8660254037844387076, 1.000000000000000000, 0.8660254037844387076, 1.000000000000000000, 0.8660254037844387076, 1.000000000000000000, 0.8660254037844387076, 1.000000000000000000, 0.8660254037844387076, 1.000000000000000000, 0.8660254037844387076, 1.000000000000000000, 0.8660254037844387076, 1.000000000000000000, 0.8660254037844387076, 1.000000000000000000, 0.8660254037844387076, 1.000000000000000000, 0.8660254037844387076, 1.000000000000000000, 0.8660254037844387076, 1.000000000000000000, 0.8660254037844387076, 1.000000000000000000, 0.8660254037844387076, 1.000000000000000000, 0.8660254037844387076, 1.000000000000000000, 0.8660254037844387076, 1.000000000000000000, 0.8660254037844387076, 1.000000000000000000, 0.8660254037844387076, 1.000000000000000000, 0.8660254037844387076, 1.000000000000000000, 0.8660254037844387076, 1.000000000000000000, 0.8660254037844387076, 1.000000000000000000, 0.8660254037844387076, 1.000000000000000000, 0.8660254037844387076, 1.000000000000000000, 0.8660254037844387076, 1.000000000000000000, 0.8660254037844387076, 1.000000000000000000, 0.8660254037844387076, 1.000000000000000000, 0.8660254037844387076, 1.000000000000000000, 0.8660254037844387076, 1.000000000000000000, 0.8660254037844387076, 1.000000000000000000, 0.8660254037844387076, 1.000000000000000000, 0.8660254037844387076, 1.000000000000000000, 0.9593432414028981725, 0.9433623850486876350 ) ) 
 REPRESENTATION_ITEM ( '' )  );
#3947 = CARTESIAN_POINT ( 'NONE',  ( -79.64356964374998427, -34.49062499938548854, 98.40857419181659793 ) ) ;
#3948 = CARTESIAN_POINT ( 'NONE',  ( -83.77821517812500929, -34.67812499938548854, -97.61286128772489690 ) ) ;
#3949 = CARTESIAN_POINT ( 'NONE',  ( 82.39999999999999147, -32.27812499938548285, 96.81714838363319586 ) ) ;
#3950 = PRODUCT_DEFINITION_FORMATION_WITH_SPECIFIED_SOURCE ( 'ANY', '', #2493, .NOT_KNOWN. ) ;
#3951 = CARTESIAN_POINT ( 'NONE',  ( 83.77821517812500929, -33.02812499938548285, -97.61286128772489690 ) ) ;
#3952 = CARTESIAN_POINT ( 'NONE',  ( 235.3564303562499447, -32.20312499938548001, -48.40857419181671162 ) ) ;
#3953 = CARTESIAN_POINT ( 'NONE',  ( -85.15643035625001289, -33.74062499938548854, 99.99999999999998579 ) ) ;
#3954 = CARTESIAN_POINT ( 'NONE',  ( 81.02178482187500208, -31.34062499938548996, -102.3871387122750889 ) ) ;
#3955 = ORIENTED_EDGE ( 'NONE', *, *, #7675, .T. ) ;
#3956 = CARTESIAN_POINT ( 'NONE',  ( 79.64356964375001269, -34.94062499938549138, 101.5914258081833879 ) ) ;
#3957 = CARTESIAN_POINT ( 'NONE',  ( 111.5000000000000142, 12.69999999999998508, 112.0000000000000142 ) ) ;
#3958 = CARTESIAN_POINT ( 'NONE',  ( -82.39999999999999147, -34.61250000000000426, 96.53589838486223584 ) ) ;
#3959 = CARTESIAN_POINT ( 'NONE',  ( -79.64356964375001269, -33.10312499938549280, 101.5914258081833879 ) ) ;
#3960 = CARTESIAN_POINT ( 'NONE',  ( -79.64356964374999848, -31.71562499938548285, 99.99999999999998579 ) ) ;
#3961 = DIRECTION ( 'NONE',  ( 1.000000000000000000, -5.139921410301648824E-16, 1.621047990368529987E-30 ) ) ;
#3962 = ADVANCED_FACE ( 'NONE', ( #18893 ), #12402, .T. ) ;
#3963 = CARTESIAN_POINT ( 'NONE',  ( 229.8435696437499587, -33.32812499938548001, 98.40857419181659793 ) ) ;
#3964 = CARTESIAN_POINT ( 'NONE',  ( -82.40000000000000568, -30.11250000000000071, 96.99999999999998579 ) ) ;
#3965 = CARTESIAN_POINT ( 'NONE',  ( -85.40000000000000568, -29.99606250001229313, 99.99999999999998579 ) ) ;
#3966 = VECTOR ( 'NONE', #6825, 1000.000000000000000 ) ;
#3967 = CARTESIAN_POINT ( 'NONE',  ( 3.878096787214571073, 2.680238624820943549, -2.357690525401585191 ) ) ;
#3968 = CARTESIAN_POINT ( 'NONE',  ( 4.175813232069148562, 4.122719923832742772, -5.545971589517866732E-16 ) ) ;
#3969 = CARTESIAN_POINT ( 'NONE',  ( -85.15643035624999868, -30.62812499938548427, 98.40857419181659793 ) ) ;
#3970 = CARTESIAN_POINT ( 'NONE',  ( -79.39999999999999147, -32.38124999877096855, -101.7320508075688963 ) ) ;
#3971 = CARTESIAN_POINT ( 'NONE',  ( 232.5999999999999375, -29.99999999999999645, -47.00000000000010658 ) ) ;
#3972 = CARTESIAN_POINT ( 'NONE',  ( 234.7581833435467047, -32.00000000000000000, 97.97695283456471316 ) ) ;
#3973 = AXIS2_PLACEMENT_3D ( 'NONE', #4322, #10283, #4415 ) ;
#3974 = CARTESIAN_POINT ( 'NONE',  ( -82.40000000000000568, -30.00000000000000355, 103.0000000000000000 ) ) ;
#3975 = CARTESIAN_POINT ( 'NONE',  ( 79.64356964375001269, -34.94062499938549138, -98.40857419181659793 ) ) ;
#3976 = CARTESIAN_POINT ( 'NONE',  ( 4.175813232069147674, 2.061359961916367833, 3.570380186727398097 ) ) ;
#3977 = ADVANCED_FACE ( 'NONE', ( #2370 ), #8331, .T. ) ;
#3978 = EDGE_CURVE ( 'NONE', #15550, #2447, #4545, .T. ) ;
#3979 = ORIENTED_EDGE ( 'NONE', *, *, #8908, .T. ) ;
#3980 = CARTESIAN_POINT ( 'NONE',  ( 79.39999999999999147, -32.41874999877096997, 99.99999999999998579 ) ) ;
#3981 = CARTESIAN_POINT ( 'NONE',  ( 235.0940413310670465, -34.99999999999998579, -48.81289630734742246 ) ) ;
#3982 = CARTESIAN_POINT ( 'NONE',  ( 229.8435696437499303, -32.50312499938547717, -50.00000000000011369 ) ) ;
#3983 = CIRCLE ( 'NONE', #565, 2.200000000000007283 ) ;
#3984 =( BOUNDED_CURVE ( )  B_SPLINE_CURVE ( 2, ( #14323, #4171, #9743, #14414, #7101 ),
 .UNSPECIFIED., .F., .F. ) 
 B_SPLINE_CURVE_WITH_KNOTS ( ( 3, 2, 3 ),
 ( 0.2975293541897499061, 0.3055555555555555802, 0.3125000000000000555 ),
 .UNSPECIFIED. ) 
 CURVE ( )  GEOMETRIC_REPRESENTATION_ITEM ( )  RATIONAL_B_SPLINE_CURVE ( ( 0.9346381638529874802, 0.9225778897267407075, 1.000000000000000000, 0.9330127018922187432, 0.9330127018922192983 ) ) 
 REPRESENTATION_ITEM ( '' )  );
#3985 = CARTESIAN_POINT ( 'NONE',  ( 85.40000000000000568, -34.53750000000000142, 101.7320508075688821 ) ) ;
#3986 = LINE ( 'NONE', #14426, #6820 ) ;
#3987 = ORIENTED_EDGE ( 'NONE', *, *, #9704, .T. ) ;
#3988 = CARTESIAN_POINT ( 'NONE',  ( -85.15643035625001289, -32.39062499938548711, -99.99999999999998579 ) ) ;
#3989 = DIRECTION ( 'NONE',  ( -0.000000000000000000, -0.000000000000000000, -1.000000000000000000 ) ) ;
#3990 = EDGE_CURVE ( 'NONE', #3532, #18754, #8811, .T. ) ;
#3991 = ORIENTED_EDGE ( 'NONE', *, *, #7428, .T. ) ;
#3992 = CARTESIAN_POINT ( 'NONE',  ( 79.64356964374999848, -34.07812499938548711, 99.99999999999998579 ) ) ;
#3993 = AXIS2_PLACEMENT_3D ( 'NONE', #17952, #10421, #11693 ) ;
#3994 = CARTESIAN_POINT ( 'NONE',  ( -85.40000000000000568, -35.36739044046696279, -101.0919052301551204 ) ) ;
#3995 = CARTESIAN_POINT ( 'NONE',  ( 85.40000000000000568, -33.60000000000000142, 99.99999999999998579 ) ) ;
#3996 = CARTESIAN_POINT ( 'NONE',  ( 81.59615242270662350, -34.57634618820329564, -96.99999999999997158 ) ) ;
#3997 = CARTESIAN_POINT ( 'NONE',  ( -85.40000000000000568, -33.50624999877096855, 101.7320508075688679 ) ) ;
#3998 = CARTESIAN_POINT ( 'NONE',  ( -83.77821517812500929, -30.32812499938548711, 97.61286128772489690 ) ) ;
#3999 = AXIS2_PLACEMENT_3D ( 'NONE', #16398, #4385, #16215 ) ;
#4000 = CARTESIAN_POINT ( 'NONE',  ( -83.77821517812500929, -32.01562499938548001, -102.3871387122750889 ) ) ;
#4001 = VECTOR ( 'NONE', #7169, 1000.000000000000000 ) ;
#4002 = FACE_OUTER_BOUND ( 'NONE', #16942, .T. ) ;
#4003 = CARTESIAN_POINT ( 'NONE',  ( 85.40000000000000568, -31.74374999877096926, -99.99999999999998579 ) ) ;
#4004 = CARTESIAN_POINT ( 'NONE',  ( 232.5999999999999375, -30.78749999999999432, 103.4641016151377499 ) ) ;
#4005 = EDGE_CURVE ( 'NONE', #13667, #13807, #12725, .T. ) ;
#4006 = VERTEX_POINT ( 'NONE', #15154 ) ;
#4007 = CARTESIAN_POINT ( 'NONE',  ( 113.0000000000000000, 10.39615242270649453, -145.0000000000000000 ) ) ;
#4008 = CONICAL_SURFACE ( 'NONE', #1517, 5.371010071662833063, 1.221730476396037490 ) ;
#4009 = PRESENTATION_STYLE_ASSIGNMENT (( #1274 ) ) ;
#4010 = CARTESIAN_POINT ( 'NONE',  ( 232.5999999999999375, -32.30624999877095860, 96.53589838486223584 ) ) ;
#4011 = CARTESIAN_POINT ( 'NONE',  ( 235.5999999999999943, -31.03124999877096357, -51.73205080756900287 ) ) ;
#4012 = ADVANCED_FACE ( 'NONE', ( #16245 ), #1681, .T. ) ;
#4013 = CARTESIAN_POINT ( 'NONE',  ( -84.44489485864974654, -35.00000000000000000, 97.76983701218843237 ) ) ;
#4014 = CARTESIAN_POINT ( 'NONE',  ( -79.64356964374998427, -30.32812499938548711, 98.40857419181659793 ) ) ;
#4015 = ORIENTED_EDGE ( 'NONE', *, *, #15676, .T. ) ;
#4016 = EDGE_LOOP ( 'NONE', ( #8880, #9781, #1377, #1515 ) ) ;
#4017 = CARTESIAN_POINT ( 'NONE',  ( -82.40000000000000568, -32.08124999877097139, 102.9999999999999858 ) ) ;
#4018 = AXIS2_PLACEMENT_3D ( 'NONE', #9893, #3732, #9697 ) ;
#4019 = DIRECTION ( 'NONE',  ( -1.000000000000000000, 4.625929269271494788E-16, 0.000000000000000000 ) ) ;
#4020 = VERTEX_POINT ( 'NONE', #1395 ) ;
#4021 = PRESENTATION_STYLE_ASSIGNMENT (( #11540 ) ) ;
#4022 = CARTESIAN_POINT ( 'NONE',  ( 83.90000000000000568, -32.77499999999999858, -97.40192378864668399 ) ) ;
#4023 = CARTESIAN_POINT ( 'NONE',  ( 80.24533121543018410, -31.99999999999997868, -102.0417045141622339 ) ) ;
#4024 = CARTESIAN_POINT ( 'NONE',  ( -82.39999999999999147, -31.94062499938548427, 103.1828516163667899 ) ) ;
#4025 = CARTESIAN_POINT ( 'NONE',  ( -80.90000000000000568, -33.30000000000000426, 97.40192378864668399 ) ) ;
#4026 = EDGE_CURVE ( 'NONE', #17606, #11560, #10534, .T. ) ;
#4027 = DIRECTION ( 'NONE',  ( -0.000000000000000000, -1.000000000000000000, -0.000000000000000000 ) ) ;
#4028 = LINE ( 'NONE', #11731, #2567 ) ;
#4029 = CARTESIAN_POINT ( 'NONE',  ( 81.02178482187500208, -34.45312499938548711, -97.61286128772489690 ) ) ;
#4030 = CARTESIAN_POINT ( 'NONE',  ( 232.5999999999999375, -33.65624999877096002, -53.00000000000011369 ) ) ;
#4031 = CARTESIAN_POINT ( 'NONE',  ( -82.39999999999999147, -34.97812499938547859, 103.1828516163667899 ) ) ;
#4032 = LINE ( 'NONE', #2365, #11774 ) ;
#4033 = EDGE_LOOP ( 'NONE', ( #14337, #18163, #9294, #4682 ) ) ;
#4034 = CARTESIAN_POINT ( 'NONE',  ( 231.0999999999999375, -34.87499999999999289, -47.40192378864679768 ) ) ;
#4035 = CARTESIAN_POINT ( 'NONE',  ( 235.3288510558096505, -35.00000000000001421, 99.22311565912356457 ) ) ;
#4036 = DIRECTION ( 'NONE',  ( 0.000000000000000000, 0.000000000000000000, -1.000000000000000000 ) ) ;
#4037 =( BOUNDED_CURVE ( )  B_SPLINE_CURVE ( 2, ( #16720, #2057, #613, #6562, #5100, #18579, #8014, #13689, #5007 ),
 .UNSPECIFIED., .F., .F. ) 
 B_SPLINE_CURVE_WITH_KNOTS ( ( 3, 2, 2, 2, 3 ),
 ( 0.5625000000000000000, 0.5694444444444444198, 0.5833333333333333703, 0.5972222222222222099, 0.6041666666666665186 ),
 .UNSPECIFIED. ) 
 CURVE ( )  GEOMETRIC_REPRESENTATION_ITEM ( )  RATIONAL_B_SPLINE_CURVE ( ( 0.9330127018922194093, 0.9330127018922194093, 1.000000000000000000, 0.8660254037844387076, 1.000000000000000000, 0.8660254037844387076, 1.000000000000000000, 0.9330127018922209636, 0.9330127018922194093 ) ) 
 REPRESENTATION_ITEM ( '' )  );
#4038 = CARTESIAN_POINT ( 'NONE',  ( 249.9999999999999716, -5.000000000000004441, -100.0000000000000000 ) ) ;
#4039 = CARTESIAN_POINT ( 'NONE',  ( -85.15643035624999868, -34.34062499938548285, 98.40857419181659793 ) ) ;
#4040 = EDGE_CURVE ( 'NONE', #1717, #7460, #6182, .T. ) ;
#4041 = CARTESIAN_POINT ( 'NONE',  ( 233.9782151781249411, -35.05312499938548143, -47.61286128772501769 ) ) ;
#4042 = ORIENTED_EDGE ( 'NONE', *, *, #9244, .F. ) ;
#4043 = CARTESIAN_POINT ( 'NONE',  ( -85.15643035624999868, -34.15312499938548285, 101.5914258081833879 ) ) ;
#4044 = CARTESIAN_POINT ( 'NONE',  ( -84.70388354820684640, -35.00002705695768412, -101.9214814096701076 ) ) ;
#4045 = CARTESIAN_POINT ( 'NONE',  ( 85.15643035624999868, -34.67812499938548143, 101.5914258081833879 ) ) ;
#4046 = CARTESIAN_POINT ( 'NONE',  ( -2.245091464683528031E-15, 3.375361811986501870, -1.153701847711632089 ) ) ;
#4047 = CARTESIAN_POINT ( 'NONE',  ( 235.3564303562499447, -30.36562499938547788, 99.99999999999998579 ) ) ;
#4048 = CARTESIAN_POINT ( 'NONE',  ( 229.8435696437499303, -32.84062499938547575, -50.00000000000011369 ) ) ;
#4049 = CARTESIAN_POINT ( 'NONE',  ( -79.64356964374998427, -35.01562499938548711, 101.5914258081833879 ) ) ;
#4050 = CARTESIAN_POINT ( 'NONE',  ( -82.39999999999999147, -34.41562499938548569, -103.1828516163667899 ) ) ;
#4051 = CARTESIAN_POINT ( 'NONE',  ( 85.15643035624999868, -33.25312499938548427, 98.40857419181659793 ) ) ;
#4052 = CARTESIAN_POINT ( 'NONE',  ( 79.64356964375001269, -34.04062499938549280, -98.40857419181659793 ) ) ;
#4053 = CARTESIAN_POINT ( 'NONE',  ( 233.9782151781249411, -33.14062499938548001, -47.61286128772501769 ) ) ;
#4054 = CARTESIAN_POINT ( 'NONE',  ( -81.02178482187500208, -33.89062499938548711, 97.61286128772489690 ) ) ;
#4055 = CARTESIAN_POINT ( 'NONE',  ( 85.15643035625001289, -31.04062499938548569, -99.99999999999998579 ) ) ;
#4056 = EDGE_LOOP ( 'NONE', ( #9724, #11835, #9144, #298 ) ) ;
#4057 = DIRECTION ( 'NONE',  ( 0.000000000000000000, 0.000000000000000000, -1.000000000000000000 ) ) ;
#4058 = CARTESIAN_POINT ( 'NONE',  ( 4.071447262713887127, 2.020725942163688504, 3.500000000000000000 ) ) ;
#4059 = CARTESIAN_POINT ( 'NONE',  ( -79.39999999999999147, -34.68750000000000000, 98.26794919243110371 ) ) ;
#4060 = CARTESIAN_POINT ( 'NONE',  ( -82.39999999999999147, -34.07812499938548711, 103.1828516163667899 ) ) ;
#4061 = CARTESIAN_POINT ( 'NONE',  ( -85.15643035625001289, -30.59062499938548285, 99.99999999999998579 ) ) ;
#4062 = EDGE_LOOP ( 'NONE', ( #14614, #10676, #16220, #18509 ) ) ;
#4063 = CARTESIAN_POINT ( 'NONE',  ( 232.5999999999999091, -32.08124999877096428, 102.9999999999999858 ) ) ;
#4064 = PRODUCT_DEFINITION_SHAPE ( 'NONE', 'NONE',  #19326 ) ;
#4066 = CARTESIAN_POINT ( 'NONE',  ( 233.9782151781249411, -33.59062499938547575, 102.3871387122750889 ) ) ;
#4065 =( BOUNDED_CURVE ( )  B_SPLINE_CURVE ( 2, ( #5298, #11440, #11244, #18481, #3721, #9782, #18774, #17306, #3912 ),
 .UNSPECIFIED., .F., .F. ) 
 B_SPLINE_CURVE_WITH_KNOTS ( ( 3, 2, 2, 2, 3 ),
 ( 0.6458333333333333703, 0.6527777777777777901, 0.6666666666666666297, 0.6805555555555555802, 0.6875000000000000000 ),
 .UNSPECIFIED. ) 
 CURVE ( )  GEOMETRIC_REPRESENTATION_ITEM ( )  RATIONAL_B_SPLINE_CURVE ( ( 0.9330127018922192983, 0.9330127018922198534, 1.000000000000000000, 0.8660254037844387076, 1.000000000000000000, 0.8660254037844387076, 1.000000000000000000, 0.9330127018922194093, 0.9330127018922194093 ) ) 
 REPRESENTATION_ITEM ( '' )  );
#4067 = LINE ( 'NONE', #7186, #12652 ) ;
#4068 = CARTESIAN_POINT ( 'NONE',  ( 1.391697335622810172, 4.043246145443375461, -3.503898532754365913 ) ) ;
#4069 = CARTESIAN_POINT ( 'NONE',  ( -85.40000000000000568, -34.93124999877096570, 98.26794919243111792 ) ) ;
#4070 = CARTESIAN_POINT ( 'NONE',  ( -80.90000000000000568, -33.39374999877097139, -97.40192378864668399 ) ) ;
#4071 = DIRECTION ( 'NONE',  ( -0.000000000000000000, -0.000000000000000000, -1.000000000000000000 ) ) ;
#4072 = CARTESIAN_POINT ( 'NONE',  ( 79.64356964375001269, -30.44062499938548783, 101.5914258081833879 ) ) ;
#4073 = CARTESIAN_POINT ( 'NONE',  ( -83.20395887649183919, -35.00000000000001421, -97.36341917746362640 ) ) ;
#4074 = CARTESIAN_POINT ( 'NONE',  ( -85.40000000000000568, -32.68124999877097281, -101.7320508075688821 ) ) ;
#4075 = CARTESIAN_POINT ( 'NONE',  ( 82.39999999999999147, -34.19062499938548427, -103.1828516163667899 ) ) ;
#4076 = CARTESIAN_POINT ( 'NONE',  ( -85.40000000000000568, -33.05624999877097281, 101.7320508075688821 ) ) ;
#4077 = ORIENTED_EDGE ( 'NONE', *, *, #1230, .T. ) ;
#4078 = CARTESIAN_POINT ( 'NONE',  ( 85.40000000000000568, -33.95624999877097139, 98.26794919243111792 ) ) ;
#4079 = CARTESIAN_POINT ( 'NONE',  ( 232.5999999999999375, -34.64062499938548001, 103.1828516163667899 ) ) ;
#4080 = CARTESIAN_POINT ( 'NONE',  ( 229.8435696437499303, -32.95312499938548001, -50.00000000000011369 ) ) ;
#4081 = CYLINDRICAL_SURFACE ( 'NONE', #580, 3.000000000000002665 ) ;
#4082 = CARTESIAN_POINT ( 'NONE',  ( 3.806834918298647619, -3.031088913245542749, -1.750000000000000222 ) ) ;
#4083 = EDGE_LOOP ( 'NONE', ( #12988, #12112, #208, #13069 ) ) ;
#4084 = CARTESIAN_POINT ( 'NONE',  ( -83.77821517812500929, -33.21562499938548285, -97.61286128772489690 ) ) ;
#4085 = CARTESIAN_POINT ( 'NONE',  ( -82.40000000000000568, -30.00000000000000355, 99.99999999999998579 ) ) ;
#4086 = EDGE_LOOP ( 'NONE', ( #9878, #19172, #19075, #15593 ) ) ;
#4087 = CARTESIAN_POINT ( 'NONE',  ( 100.0000000000000000, 10.19999999999997620, -139.9999999999999716 ) ) ;
#4088 = CARTESIAN_POINT ( 'NONE',  ( -85.15643035624999868, -32.01562499938548711, -98.40857419181659793 ) ) ;
#4089 = CARTESIAN_POINT ( 'NONE',  ( 82.39999999999999147, -33.48750000000000426, 96.53589838486223584 ) ) ;
#4090 = CARTESIAN_POINT ( 'NONE',  ( -85.40000000000000568, -34.46249999999999858, 101.7320508075688821 ) ) ;
#4091 = CARTESIAN_POINT ( 'NONE',  ( -82.39999999999999147, -34.78124999877096712, 103.4641016151377499 ) ) ;
#4092 = CARTESIAN_POINT ( 'NONE',  ( -85.15643035624999868, -31.19062499938548783, 98.40857419181659793 ) ) ;
#4093 = CARTESIAN_POINT ( 'NONE',  ( -81.02178482187500208, -33.14062499938548711, -97.61286128772489690 ) ) ;
#4094 = EDGE_CURVE ( 'NONE', #10447, #14621, #17807, .T. ) ;
#4095 = CARTESIAN_POINT ( 'NONE',  ( 232.5002178375172832, -34.99999999999998579, 102.7603866155199199 ) ) ;
#4096 = CARTESIAN_POINT ( 'NONE',  ( 85.40000000000000568, -31.29374999877096997, -99.99999999999998579 ) ) ;
#4097 = CARTESIAN_POINT ( 'NONE',  ( 229.5999999999999375, -30.86249999999999361, 101.7320508075688679 ) ) ;
#4098 =( BOUNDED_CURVE ( )  B_SPLINE_CURVE ( 2, ( #13861, #503, #16906, #16812, #6456, #18669, #15336, #14063, #2153 ),
 .UNSPECIFIED., .F., .F. ) 
 B_SPLINE_CURVE_WITH_KNOTS ( ( 3, 2, 2, 2, 3 ),
 ( 0.3541666666666666852, 0.3611111111111111049, 0.3750000000000000000, 0.3888888888888888951, 0.3958333333333333703 ),
 .UNSPECIFIED. ) 
 CURVE ( )  GEOMETRIC_REPRESENTATION_ITEM ( )  RATIONAL_B_SPLINE_CURVE ( ( 0.9330127018922194093, 0.9330127018922196314, 1.000000000000000000, 0.8660254037844387076, 1.000000000000000000, 0.8660254037844387076, 1.000000000000000000, 0.9330127018922190762, 0.9330127018922194093 ) ) 
 REPRESENTATION_ITEM ( '' )  );
#4099 = EDGE_CURVE ( 'NONE', #18958, #8738, #3135, .T. ) ;
#4100 = ORIENTED_EDGE ( 'NONE', *, *, #4005, .T. ) ;
#4101 = CARTESIAN_POINT ( 'NONE',  ( 229.8435696437499587, -32.02817623523064583, -48.94122380911299075 ) ) ;
#4102 = FILL_AREA_STYLE_COLOUR ( '', #3630 ) ;
#4103 = CARTESIAN_POINT ( 'NONE',  ( 231.0999999999999375, -33.46874999877096002, 102.5980762113533018 ) ) ;
#4104 = CARTESIAN_POINT ( 'NONE',  ( 235.5999999999999943, -30.58124999877096073, -51.73205080756900287 ) ) ;
#4105 = CARTESIAN_POINT ( 'NONE',  ( -82.65380294351676582, -34.99990492518305274, 97.01075526832239859 ) ) ;
#4106 = CARTESIAN_POINT ( 'NONE',  ( -82.39999999999999147, -31.60312499938548569, 96.81714838363319586 ) ) ;
#4107 = ORIENTED_EDGE ( 'NONE', *, *, #7315, .F. ) ;
#4108 = ORIENTED_EDGE ( 'NONE', *, *, #9892, .T. ) ;
#4109 = DIRECTION ( 'NONE',  ( -1.000000000000000000, -0.000000000000000000, -0.000000000000000000 ) ) ;
#4110 = CARTESIAN_POINT ( 'NONE',  ( 234.0999999999999375, -34.35000000000000142, -47.40192378864679768 ) ) ;
#4111 = ORIENTED_EDGE ( 'NONE', *, *, #1604, .T. ) ;
#4112 = DIRECTION ( 'NONE',  ( -1.000000000000000000, 0.000000000000000000, 0.000000000000000000 ) ) ;
#4113 = CARTESIAN_POINT ( 'NONE',  ( 79.39999999999999147, -32.02500000000000568, -99.99999999999998579 ) ) ;
#4114 = CARTESIAN_POINT ( 'NONE',  ( -4.000000000000000000, -2.309401076758512694, -3.433295621305382461 ) ) ;
#4115 = EDGE_CURVE ( 'NONE', #14649, #4852, #227, .T. ) ;
#4116 = CARTESIAN_POINT ( 'NONE',  ( -83.77821517812500929, -30.62812499938548783, 102.3871387122750889 ) ) ;
#4117 = CARTESIAN_POINT ( 'NONE',  ( -85.40000000000000568, -31.80000000000000071, 99.99999999999998579 ) ) ;
#4118 = CARTESIAN_POINT ( 'NONE',  ( -79.39999999999999147, -34.72500000000000142, -99.99999999999998579 ) ) ;
#4119 = EDGE_CURVE ( 'NONE', #6709, #531, #12017, .T. ) ;
#4120 = CARTESIAN_POINT ( 'NONE',  ( 231.0999999999999375, -32.26874999877096428, -52.59807621135342970 ) ) ;
#4121 = CARTESIAN_POINT ( 'NONE',  ( 94.79999999999991189, -3.000000000000000000, 150.0000000000000000 ) ) ;
#4122 = CARTESIAN_POINT ( 'NONE',  ( 85.23110191009456571, -35.00000000000000000, 100.8575180188180269 ) ) ;
#4123 = CARTESIAN_POINT ( 'NONE',  ( 85.15643035624999868, -35.11426555956768425, -98.99674139749697588 ) ) ;
#4124 = ORIENTED_EDGE ( 'NONE', *, *, #3421, .T. ) ;
#4125 = FILL_AREA_STYLE ('',( #13106 ) ) ;
#4126 = CARTESIAN_POINT ( 'NONE',  ( -85.15643035624999868, -31.90312499938548285, -98.40857419181659793 ) ) ;
#4127 = LINE ( 'NONE', #14187, #880 ) ;
#4128 = AXIS2_PLACEMENT_3D ( 'NONE', #18082, #3022, #12010 ) ;
#4129 = AXIS2_PLACEMENT_3D ( 'NONE', #1468, #16030, #2632 ) ;
#4130 = CARTESIAN_POINT ( 'NONE',  ( 232.5999999999999375, -29.99999999999999645, 103.0000000000000000 ) ) ;
#4131 = CARTESIAN_POINT ( 'NONE',  ( 229.8435696437499587, -33.81562499938547717, 101.5914258081833879 ) ) ;
#4132 = CARTESIAN_POINT ( 'NONE',  ( -83.77821517812500929, -33.92812499938548854, 97.61286128772489690 ) ) ;
#4133 = CARTESIAN_POINT ( 'NONE',  ( 110.9999999999999574, -21.80000000000003268, -137.3499999999999943 ) ) ;
#4134 = CARTESIAN_POINT ( 'NONE',  ( 232.5999999999999375, -31.15312499938547930, -53.18285161636690361 ) ) ;
#4135 = ORIENTED_EDGE ( 'NONE', *, *, #3489, .F. ) ;
#4136 = CARTESIAN_POINT ( 'NONE',  ( -85.15643035625001289, -33.29062499938547859, 99.99999999999998579 ) ) ;
#4137 = CARTESIAN_POINT ( 'NONE',  ( -84.57144699476174310, -35.00000000000000000, -102.0792695867486657 ) ) ;
#4138 = CARTESIAN_POINT ( 'NONE',  ( 85.40000000000000568, -30.45000000000000284, 99.99999999999998579 ) ) ;
#4139 = CARTESIAN_POINT ( 'NONE',  ( 96.99999999999994316, -21.80000000000003268, -142.6499999999999773 ) ) ;
#4141 = VECTOR ( 'NONE', #6550, 1000.000000000000000 ) ;
#4140 = CARTESIAN_POINT ( 'NONE',  ( 233.9782151781249411, -32.24062499938548143, 102.3871387122750889 ) ) ;
#4142 = VECTOR ( 'NONE', #9971, 1000.000000000000000 ) ;
#4143 = CARTESIAN_POINT ( 'NONE',  ( 82.40000000000000568, -30.00000000000000355, 103.0000000000000000 ) ) ;
#4144 = EDGE_CURVE ( 'NONE', #7899, #2374, #9811, .T. ) ;
#4145 = PLANE ( 'NONE',  #12067 ) ;
#4146 = CARTESIAN_POINT ( 'NONE',  ( -85.15643035625001289, -33.36562499938548854, -98.40857419181659793 ) ) ;
#4147 = DIRECTION ( 'NONE',  ( 0.000000000000000000, 0.000000000000000000, 1.000000000000000000 ) ) ;
#4148 = CARTESIAN_POINT ( 'NONE',  ( 83.77821517812500929, -34.22812499938549280, -102.3871387122750889 ) ) ;
#4149 = CARTESIAN_POINT ( 'NONE',  ( 229.5999999999999375, -30.89999999999999858, -50.00000000000011369 ) ) ;
#4150 = CARTESIAN_POINT ( 'NONE',  ( -82.39999999999999147, -34.30312499938548143, 96.81714838363319586 ) ) ;
#4151 = CARTESIAN_POINT ( 'NONE',  ( 85.15643035624999868, -30.55312499938548854, -101.5914258081833879 ) ) ;
#4152 = ORIENTED_EDGE ( 'NONE', *, *, #10678, .T. ) ;
#4153 = CARTESIAN_POINT ( 'NONE',  ( 85.15643035625001289, -35.22676544108147567, 101.0032535741825654 ) ) ;
#4154 = CARTESIAN_POINT ( 'NONE',  ( 4.000000000000000000, -2.309401076758514915, -5.000000000000000000 ) ) ;
#4155 = EDGE_CURVE ( 'NONE', #6638, #14213, #1885, .T. ) ;
#4156 = CARTESIAN_POINT ( 'NONE',  ( -85.40000000000000568, -33.60000000000000142, 99.99999999999998579 ) ) ;
#4157 = VECTOR ( 'NONE', #16971, 1000.000000000000000 ) ;
#4158 =( BOUNDED_CURVE ( )  B_SPLINE_CURVE ( 2, ( #12461, #1911, #3473, #4666, #10615, #15399, #16867, #3184, #16674 ),
 .UNSPECIFIED., .F., .F. ) 
 B_SPLINE_CURVE_WITH_KNOTS ( ( 3, 2, 2, 2, 3 ),
 ( 0.4791666666666666297, 0.4861111111111111049, 0.5000000000000000000, 0.5138888888888888395, 0.5208333333333334814 ),
 .UNSPECIFIED. ) 
 CURVE ( )  GEOMETRIC_REPRESENTATION_ITEM ( )  RATIONAL_B_SPLINE_CURVE ( ( 0.9330127018922194093, 0.9330127018922190762, 1.000000000000000000, 0.8660254037844387076, 1.000000000000000000, 0.8660254037844387076, 1.000000000000000000, 0.9330127018922177440, 0.9330127018922194093 ) ) 
 REPRESENTATION_ITEM ( '' )  );
#4159 = CARTESIAN_POINT ( 'NONE',  ( -82.39999999999999147, -32.27812499938548285, 103.1828516163667899 ) ) ;
#4160 = CARTESIAN_POINT ( 'NONE',  ( -83.77821517812500929, -31.86562499938548498, 102.3871387122750889 ) ) ;
#4161 = ORIENTED_EDGE ( 'NONE', *, *, #1374, .T. ) ;
#4162 = CARTESIAN_POINT ( 'NONE',  ( -83.20384757729335945, -34.08615380933863293, 96.99999999999998579 ) ) ;
#4163 = CARTESIAN_POINT ( 'NONE',  ( 235.3564303562499447, -33.51562499938548001, 99.99999999999998579 ) ) ;
#4164 = DIRECTION ( 'NONE',  ( 0.000000000000000000, -1.000000000000000000, 0.000000000000000000 ) ) ;
#4165 = CARTESIAN_POINT ( 'NONE',  ( 83.20384757729335945, -33.69240381056766154, -96.99999999999998579 ) ) ;
#4166 = CARTESIAN_POINT ( 'NONE',  ( 2.804994570502171047, 3.229033611042449792, -3.526374918436834704 ) ) ;
#4167 = CARTESIAN_POINT ( 'NONE',  ( 2.691179338796023329E-15, 4.647089433458991614, -3.572167766733753691 ) ) ;
#4168 = CARTESIAN_POINT ( 'NONE',  ( 234.0999999999999375, -32.84999999999999432, 97.40192378864668399 ) ) ;
#4169 = FACE_BOUND ( 'NONE', #10381, .T. ) ;
#4170 = CARTESIAN_POINT ( 'NONE',  ( 83.77821517812500929, -33.47812499938548569, 102.3871387122750889 ) ) ;
#4171 = CARTESIAN_POINT ( 'NONE',  ( 234.9136945297046850, -32.02340763552835767, 102.1282894555902061 ) ) ;
#4172 = CARTESIAN_POINT ( 'NONE',  ( 82.39999999999999147, -32.84062499938548996, -103.1828516163667899 ) ) ;
#4173 = ORIENTED_EDGE ( 'NONE', *, *, #13656, .T. ) ;
#4174 = CARTESIAN_POINT ( 'NONE',  ( 79.39999999999999147, -31.96874999877096712, 99.99999999999998579 ) ) ;
#4175 = CONTEXT_DEPENDENT_SHAPE_REPRESENTATION ( #3837, #15601 ) ;
#4176 = CARTESIAN_POINT ( 'NONE',  ( 232.5999999999999375, -34.41562499938547859, 96.81714838363319586 ) ) ;
#4177 = CARTESIAN_POINT ( 'NONE',  ( 244.7999999999999545, -29.80000000000002203, 150.0000000000000000 ) ) ;
#4178 = DIRECTION ( 'NONE',  ( 1.000000000000000000, -0.000000000000000000, -2.407412430484046130E-31 ) ) ;
#4179 = CARTESIAN_POINT ( 'NONE',  ( -84.44763168836716716, -32.00000000000000000, 101.8452947671445799 ) ) ;
#4180 = ORIENTED_EDGE ( 'NONE', *, *, #17417, .T. ) ;
#4181 = CARTESIAN_POINT ( 'NONE',  ( -82.39999999999999147, -34.75312499938549138, -103.1828516163667899 ) ) ;
#4182 = DIRECTION ( 'NONE',  ( 0.000000000000000000, -1.000000000000000000, 0.000000000000000000 ) ) ;
#4183 = ORIENTED_EDGE ( 'NONE', *, *, #9647, .F. ) ;
#4184 = CARTESIAN_POINT ( 'NONE',  ( 79.64356964374998427, -34.94062499938548427, 101.5914258081833879 ) ) ;
#4185 = CARTESIAN_POINT ( 'NONE',  ( -85.15643035625001289, -30.70312499938548711, -99.99999999999998579 ) ) ;
#4186 = CARTESIAN_POINT ( 'NONE',  ( -83.90000000000000568, -30.91874999877096997, -102.5980762113533018 ) ) ;
#4187 = DIRECTION ( 'NONE',  ( -0.000000000000000000, 1.000000000000000000, -0.000000000000000000 ) ) ;
#4188 = CARTESIAN_POINT ( 'NONE',  ( -83.90000000000000568, -34.81874999877096855, 102.5980762113533018 ) ) ;
#4189 = CARTESIAN_POINT ( 'NONE',  ( -85.15643035625001289, -31.15312499938548996, 99.99999999999998579 ) ) ;
#4190 = CARTESIAN_POINT ( 'NONE',  ( -84.28136653320150629, -32.00000000000001421, -102.0145392219080378 ) ) ;
#4191 = CARTESIAN_POINT ( 'NONE',  ( 231.7960411235079050, -35.00000000000002132, 102.6365808225362883 ) ) ;
#4192 = CARTESIAN_POINT ( 'NONE',  ( 80.90000000000000568, -32.79374999877096997, -97.40192378864668399 ) ) ;
#4193 = CARTESIAN_POINT ( 'NONE',  ( 229.5999999999999375, -31.31249999999998934, 101.7320508075688679 ) ) ;
#4194 = ORIENTED_EDGE ( 'NONE', *, *, #16083, .T. ) ;
#4195 = CARTESIAN_POINT ( 'NONE',  ( 81.02178482187500208, -34.79062499938548569, -97.61286128772489690 ) ) ;
#4196 = SURFACE_SIDE_STYLE ('',( #13084 ) ) ;
#4197 = CARTESIAN_POINT ( 'NONE',  ( 234.0999999999999375, -32.79374999877096286, 97.40192378864668399 ) ) ;
#4198 = CARTESIAN_POINT ( 'NONE',  ( 235.5999999999999943, -32.90624999877096002, -48.26794919243124582 ) ) ;
#4199 = CARTESIAN_POINT ( 'NONE',  ( 84.44763168836732348, -32.00000000000002132, 98.15470523285560489 ) ) ;
#4200 = CARTESIAN_POINT ( 'NONE',  ( -81.02178482187500208, -32.09062499938548285, 97.61286128772489690 ) ) ;
#4201 = VERTEX_POINT ( 'NONE', #5193 ) ;
#4202 = ORIENTED_EDGE ( 'NONE', *, *, #12497, .F. ) ;
#4203 = LINE ( 'NONE', #10070, #8822 ) ;
#4204 = CARTESIAN_POINT ( 'NONE',  ( 235.5999999999999375, -34.27499999999999147, -50.00000000000011369 ) ) ;
#4205 = ORIENTED_EDGE ( 'NONE', *, *, #14141, .T. ) ;
#4206 = CARTESIAN_POINT ( 'NONE',  ( 79.39999999999999147, -32.38124999877096855, -98.26794919243110371 ) ) ;
#4207 = CARTESIAN_POINT ( 'NONE',  ( 85.40000000000000568, -33.56250000000000000, -101.7320508075688679 ) ) ;
#4208 = DIRECTION ( 'NONE',  ( 0.000000000000000000, 0.000000000000000000, -1.000000000000000000 ) ) ;
#4209 = ADVANCED_FACE ( 'NONE', ( #13783 ), #9683, .F. ) ;
#4210 = ADVANCED_FACE ( 'NONE', ( #13975 ), #1870, .F. ) ;
#4211 = CARTESIAN_POINT ( 'NONE',  ( -85.15643035624999868, -32.01562499938548711, 101.5914258081833879 ) ) ;
#4212 = CARTESIAN_POINT ( 'NONE',  ( -80.90000000000000568, -31.20000000000000284, 102.5980762113533018 ) ) ;
#4213 = CARTESIAN_POINT ( 'NONE',  ( 235.5999999999999943, -32.38124999877096144, -51.73205080756900287 ) ) ;
#4214 = CARTESIAN_POINT ( 'NONE',  ( -84.51155153715826884, -35.14114847181267720, 98.22820474807231506 ) ) ;
#4215 =( REPRESENTATION_RELATIONSHIP ('NONE','NONE', #14468, #16991 ) REPRESENTATION_RELATIONSHIP_WITH_TRANSFORMATION ( #7293 )SHAPE_REPRESENTATION_RELATIONSHIP( ) );
#4216 = CARTESIAN_POINT ( 'NONE',  ( 80.03686793005718414, -35.00000000000000000, 101.6462804658012828 ) ) ;
#4217 = PLANE ( 'NONE',  #7427 ) ;
#4218 = CARTESIAN_POINT ( 'NONE',  ( 231.7960411235079050, -35.00000000000002132, 102.6365808225362883 ) ) ;
#4219 = VERTEX_POINT ( 'NONE', #15445 ) ;
#4220 = CARTESIAN_POINT ( 'NONE',  ( -82.39999999999999147, -30.47812499938548569, -96.81714838363319586 ) ) ;
#4221 = DIRECTION ( 'NONE',  ( -0.000000000000000000, -1.000000000000000000, -0.000000000000000000 ) ) ;
#4222 = ADVANCED_FACE ( 'NONE', ( #7828 ), #18659, .T. ) ;
#4223 = AXIS2_PLACEMENT_3D ( 'NONE', #7397, #14526, #11890 ) ;
#4224 = EDGE_CURVE ( 'NONE', #6163, #16577, #10302, .T. ) ;
#4225 = CARTESIAN_POINT ( 'NONE',  ( -3.522875095019672109, 2.820352903225427532, -3.598441714920591394 ) ) ;
#4226 = CARTESIAN_POINT ( 'NONE',  ( 235.3564303562499447, -34.49062499938548143, 98.40857419181659793 ) ) ;
#4227 = CARTESIAN_POINT ( 'NONE',  ( -85.15643035624999868, -31.90312499938548285, 101.5914258081833879 ) ) ;
#4228 = CARTESIAN_POINT ( 'NONE',  ( -85.40000000000000568, -34.01250000000000284, 101.7320508075688821 ) ) ;
#4229 = CARTESIAN_POINT ( 'NONE',  ( 229.8435696437499871, -33.70312499938548001, -48.40857419181671162 ) ) ;
#4230 = ORIENTED_EDGE ( 'NONE', *, *, #3662, .T. ) ;
#4231 = ORIENTED_EDGE ( 'NONE', *, *, #11858, .T. ) ;
#4232 = CARTESIAN_POINT ( 'NONE',  ( -84.44763168836716716, -32.00000000000000000, 101.8452947671445799 ) ) ;
#4233 = CARTESIAN_POINT ( 'NONE',  ( -82.39999999999999147, -34.75312499938549138, 96.81714838363319586 ) ) ;
#4234 = EDGE_CURVE ( 'NONE', #16126, #13209, #9581, .T. ) ;
#4235 = CARTESIAN_POINT ( 'NONE',  ( -80.90000000000000568, -33.89999999999999858, -97.40192378864668399 ) ) ;
#4236 = CARTESIAN_POINT ( 'NONE',  ( 85.15643035624999868, -33.77812499938548285, 101.5914258081833879 ) ) ;
#4237 = DIRECTION ( 'NONE',  ( 1.000000000000000000, 0.000000000000000000, -0.000000000000000000 ) ) ;
#4238 = CARTESIAN_POINT ( 'NONE',  ( 231.2217848218749339, -30.96562499938547930, 102.3871387122750889 ) ) ;
#4239 = AXIS2_PLACEMENT_3D ( 'NONE', #5354, #10317, #5826 ) ;
#4240 = CARTESIAN_POINT ( 'NONE',  ( 244.7999999999999545, -32.00000000000000000, -97.80000000000002558 ) ) ;
#4241 = CARTESIAN_POINT ( 'NONE',  ( -81.59615242270662350, -30.76740381056766793, 102.9999999999999858 ) ) ;
#4242 = CARTESIAN_POINT ( 'NONE',  ( 85.40000000000000568, -33.13124999877096855, -98.26794919243111792 ) ) ;
#4243 = CARTESIAN_POINT ( 'NONE',  ( 82.39999999999999147, -31.60312499938548569, -96.81714838363319586 ) ) ;
#4244 = B_SPLINE_CURVE_WITH_KNOTS ( 'NONE', 3,
 ( #4105, #9778, #18770, #18867, #4013, #8308 ),
 .UNSPECIFIED., .F., .F.,
 ( 4, 2, 4 ),
 ( 0.5134810729395012929, 0.5761852797268253168, 0.6388894865141493407 ),
 .UNSPECIFIED. ) ;
#4245 = CARTESIAN_POINT ( 'NONE',  ( 233.9782151781249411, -34.34062499938547575, -52.38713871227520968 ) ) ;
#4246 = CARTESIAN_POINT ( 'NONE',  ( -81.02178482187500208, -32.54062499938548569, 97.61286128772489690 ) ) ;
#4247 = CARTESIAN_POINT ( 'NONE',  ( 85.15643035625001289, -30.59062499938548285, -99.99999999999998579 ) ) ;
#4248 = ORIENTED_EDGE ( 'NONE', *, *, #13454, .F. ) ;
#4249 = CARTESIAN_POINT ( 'NONE',  ( 85.15643035624999868, -34.26562499938548711, 98.40857419181659793 ) ) ;
#4250 = CARTESIAN_POINT ( 'NONE',  ( -80.90000000000000568, -34.74374999877097281, 102.5980762113533018 ) ) ;
#4251 = CARTESIAN_POINT ( 'NONE',  ( -85.39999999999999147, -34.97364041986484295, 98.90809577818232867 ) ) ;
#4252 = VECTOR ( 'NONE', #9885, 1000.000000000000000 ) ;
#4253 = CARTESIAN_POINT ( 'NONE',  ( -79.64356964375001269, -34.45312499938548711, 101.5914258081833879 ) ) ;
#4254 = ORIENTED_EDGE ( 'NONE', *, *, #9335, .T. ) ;
#4255 = CARTESIAN_POINT ( 'NONE',  ( -85.40000000000000568, -30.48749999999999716, 98.26794919243111792 ) ) ;
#4256 = CARTESIAN_POINT ( 'NONE',  ( 232.5999999999999375, -29.99999999999999645, 99.99999999999998579 ) ) ;
#4257 = CARTESIAN_POINT ( 'NONE',  ( 79.60045861139944634, -34.99999999999999289, -99.68825842090971889 ) ) ;
#4258 = CARTESIAN_POINT ( 'NONE',  ( -79.39999999999999147, -33.37106250001229313, 99.99999999999998579 ) ) ;
#4259 = FACE_OUTER_BOUND ( 'NONE', #17687, .T. ) ;
#4260 = EDGE_CURVE ( 'NONE', #17075, #2327, #9355, .T. ) ;
#4261 = CARTESIAN_POINT ( 'NONE',  ( -80.90000000000000568, -32.34374999877096712, 97.40192378864668399 ) ) ;
#4262 = CARTESIAN_POINT ( 'NONE',  ( -83.77821517812500929, -31.56562499938548427, 97.61286128772489690 ) ) ;
#4263 = CARTESIAN_POINT ( 'NONE',  ( -79.39999999999999147, -32.41874999877096997, -99.99999999999998579 ) ) ;
#4264 = CARTESIAN_POINT ( 'NONE',  ( 81.02178482187500208, -32.20312499938548711, 102.3871387122750889 ) ) ;
#4265 = CARTESIAN_POINT ( 'NONE',  ( -99.99999999999998579, 0.000000000000000000, 150.0000000000000000 ) ) ;
#4266 = CARTESIAN_POINT ( 'NONE',  ( 79.64356964374999848, -34.07812499938548711, -99.99999999999998579 ) ) ;
#4267 = FACE_OUTER_BOUND ( 'NONE', #4810, .T. ) ;
#4268 =( BOUNDED_CURVE ( )  B_SPLINE_CURVE ( 2, ( #12258, #13332, #4447, #9317, #17932, #7658, #10499, #1617, #18036 ),
 .UNSPECIFIED., .F., .F. ) 
 B_SPLINE_CURVE_WITH_KNOTS ( ( 3, 2, 2, 2, 3 ),
 ( 0.7708333333333332593, 0.7777777777777777901, 0.7916666666666666297, 0.8055555555555555802, 0.8125000000000000000 ),
 .UNSPECIFIED. ) 
 CURVE ( )  GEOMETRIC_REPRESENTATION_ITEM ( )  RATIONAL_B_SPLINE_CURVE ( ( 0.9330127018922192983, 0.9330127018922187432, 1.000000000000000000, 0.8660254037844387076, 1.000000000000000000, 0.8660254037844387076, 1.000000000000000000, 0.9330127018922194093, 0.9330127018922194093 ) ) 
 REPRESENTATION_ITEM ( '' )  );
#4269 = ORIENTED_EDGE ( 'NONE', *, *, #11640, .T. ) ;
#4270 = CARTESIAN_POINT ( 'NONE',  ( 82.39999999999999147, -34.10624999877096997, 103.4641016151377499 ) ) ;
#4271 = CARTESIAN_POINT ( 'NONE',  ( 231.7960411235079050, -35.00000000000002132, -47.36341917746382535 ) ) ;
#4272 = FACE_OUTER_BOUND ( 'NONE', #6582, .T. ) ;
#4273 = CARTESIAN_POINT ( 'NONE',  ( 232.5999999999999375, -34.33124999877097139, 102.9999999999999858 ) ) ;
#4274 = CARTESIAN_POINT ( 'NONE',  ( 232.5999999999999375, -29.99999999999999645, 96.99999999999998579 ) ) ;
#4275 = VERTEX_POINT ( 'NONE', #10852 ) ;
#4276 = CARTESIAN_POINT ( 'NONE',  ( -81.02178482187500208, -33.14062499938548711, -97.61286128772489690 ) ) ;
#4277 = AXIS2_PLACEMENT_3D ( 'NONE', #16017, #9966, #11329 ) ;
#4278 = CARTESIAN_POINT ( 'NONE',  ( 0.000000000000000000, 3.755786496842896592E-16, -3.499999999999999556 ) ) ;
#4279 = VERTEX_POINT ( 'NONE', #15645 ) ;
#4280 = CARTESIAN_POINT ( 'NONE',  ( 99.99999999999997158, -5.200000000000008171, 150.0000000000000000 ) ) ;
#4281 = CARTESIAN_POINT ( 'NONE',  ( -82.39999999999999147, -35.23124999877096997, -96.53589838486223584 ) ) ;
#4282 = CARTESIAN_POINT ( 'NONE',  ( 231.0999999999999375, -34.42499999999999716, -47.40192378864679768 ) ) ;
#4283 = CARTESIAN_POINT ( 'NONE',  ( -82.39999999999999147, -31.18124999877096926, -96.53589838486223584 ) ) ;
#4284 = CARTESIAN_POINT ( 'NONE',  ( 235.3564303562499447, -31.41562499938548214, 101.5914258081833879 ) ) ;
#4285 = CARTESIAN_POINT ( 'NONE',  ( -82.39999999999999147, -33.43124999877097281, 103.4641016151377499 ) ) ;
#4286 = AXIS2_PLACEMENT_3D ( 'NONE', #15644, #12993, #14355 ) ;
#4287 = CARTESIAN_POINT ( 'NONE',  ( -79.64356964374999848, -33.62812499938548427, 99.99999999999998579 ) ) ;
#4288 = CARTESIAN_POINT ( 'NONE',  ( -80.90000000000000568, -31.65000000000000568, 102.5980762113533018 ) ) ;
#4289 = DIRECTION ( 'NONE',  ( 1.000000000000000000, 0.000000000000000000, 0.000000000000000000 ) ) ;
#4290 = CARTESIAN_POINT ( 'NONE',  ( 232.5999999999999375, -32.36249999999999716, -53.00000000000011369 ) ) ;
#4291 = CARTESIAN_POINT ( 'NONE',  ( 83.90000000000000568, -30.76874999877097139, -102.5980762113533018 ) ) ;
#4292 = AXIS2_PLACEMENT_3D ( 'NONE', #15614, #12293, #6534 ) ;
#4293 = CARTESIAN_POINT ( 'NONE',  ( 232.5999999999999375, -33.93750000000000000, 103.4641016151377499 ) ) ;
#4294 = CONICAL_SURFACE ( 'NONE', #18974, 3.500000000000000000, 1.047197551196600296 ) ;
#4295 = EDGE_LOOP ( 'NONE', ( #18241, #4301, #3641, #18199 ) ) ;
#4296 = CARTESIAN_POINT ( 'NONE',  ( 229.5999999999999375, -33.50624999877096144, 101.7320508075688679 ) ) ;
#4297 = CARTESIAN_POINT ( 'NONE',  ( 232.5999999999999375, -34.33124999877096428, -46.53589838486234953 ) ) ;
#4298 = CARTESIAN_POINT ( 'NONE',  ( -83.77821517812500929, -34.11562499938548854, 102.3871387122750889 ) ) ;
#4299 = CIRCLE ( 'NONE', #8653, 6.000000000000015987 ) ;
#4300 = VERTEX_POINT ( 'NONE', #18580 ) ;
#4301 = ORIENTED_EDGE ( 'NONE', *, *, #15701, .T. ) ;
#4302 = PLANE ( 'NONE',  #5412 ) ;
#4303 = FACE_OUTER_BOUND ( 'NONE', #11025, .T. ) ;
#4304 = DIRECTION ( 'NONE',  ( 0.000000000000000000, 0.000000000000000000, 1.000000000000000000 ) ) ;
#4305 = ORIENTED_EDGE ( 'NONE', *, *, #8001, .F. ) ;
#4306 = CARTESIAN_POINT ( 'NONE',  ( -83.90000000000000568, -31.66874999877096997, 102.5980762113533018 ) ) ;
#4307 = CARTESIAN_POINT ( 'NONE',  ( 82.39999999999999147, -34.38750000000000284, -103.4641016151377499 ) ) ;
#4308 = CARTESIAN_POINT ( 'NONE',  ( 111.0000000000000000, 10.19999999999997620, -139.9999999999999716 ) ) ;
#4309 = AXIS2_PLACEMENT_3D ( 'NONE', #8868, #14826, #11810 ) ;
#4310 = VECTOR ( 'NONE', #13744, 999.9999999999998863 ) ;
#4311 = CARTESIAN_POINT ( 'NONE',  ( -79.64356964375001269, -34.56562499938549138, 101.5914258081833879 ) ) ;
#4312 = CARTESIAN_POINT ( 'NONE',  ( -85.40000000000000568, -32.66250000000000142, 101.7320508075688679 ) ) ;
#4313 = FACE_OUTER_BOUND ( 'NONE', #6565, .T. ) ;
#4314 = SURFACE_STYLE_FILL_AREA ( #15853 ) ;
#4315 = AXIS2_PLACEMENT_3D ( 'NONE', #15548, #11138, #9381 ) ;
#4316 = CARTESIAN_POINT ( 'NONE',  ( 79.67114894419049165, -35.00000000000001421, 100.7768843408770181 ) ) ;
#4317 = CARTESIAN_POINT ( 'NONE',  ( 84.06832524826147335, -34.99999999999999289, 97.74327260033980735 ) ) ;
#4318 = CARTESIAN_POINT ( 'NONE',  ( -85.40000000000000568, -34.46249999999999858, -98.26794919243111792 ) ) ;
#4319 = ORIENTED_EDGE ( 'NONE', *, *, #11532, .F. ) ;
#4320 = SURFACE_SIDE_STYLE ('',( #14561 ) ) ;
#4321 = CARTESIAN_POINT ( 'NONE',  ( -79.64356964374999848, -30.81562499938548427, -99.99999999999998579 ) ) ;
#4322 = CARTESIAN_POINT ( 'NONE',  ( 111.5000000000000142, 12.69999999999998508, 50.00000000000001421 ) ) ;
#4323 = VECTOR ( 'NONE', #18883, 1000.000000000000000 ) ;
#4324 = CARTESIAN_POINT ( 'NONE',  ( 234.0999999999999375, -34.74374999877096570, -47.40192378864679768 ) ) ;
#4325 = CARTESIAN_POINT ( 'NONE',  ( -83.20384757729337366, -32.55134618820330417, 103.0000000000000000 ) ) ;
#4326 = CARTESIAN_POINT ( 'NONE',  ( -83.77821517812500929, -30.21562499938548285, 97.61286128772489690 ) ) ;
#4327 = CARTESIAN_POINT ( 'NONE',  ( 82.39999999999999147, -32.81250000000000000, 103.0000000000000000 ) ) ;
#4328 = CARTESIAN_POINT ( 'NONE',  ( 235.3564303562499447, -34.00312499938547717, -48.40857419181671162 ) ) ;
#4329 = EDGE_LOOP ( 'NONE', ( #10415, #13849, #5051, #7916 ) ) ;
#4330 = ORIENTED_EDGE ( 'NONE', *, *, #9496, .T. ) ;
#4331 = CARTESIAN_POINT ( 'NONE',  ( -84.74067385206564040, -32.00000000000000711, 98.53339280468568973 ) ) ;
#4332 = CARTESIAN_POINT ( 'NONE',  ( -85.40000000000000568, -30.45000000000000284, 99.99999999999998579 ) ) ;
#4333 = CARTESIAN_POINT ( 'NONE',  ( 82.40000000000000568, -32.08124999877097139, -102.9999999999999858 ) ) ;
#4334 = CARTESIAN_POINT ( 'NONE',  ( 83.77821517812500929, -33.81562499938548427, 102.3871387122750889 ) ) ;
#4335 = CARTESIAN_POINT ( 'NONE',  ( 232.5999999999999375, -33.20624999877097139, -53.00000000000011369 ) ) ;
#4336 = CARTESIAN_POINT ( 'NONE',  ( 232.5999999999999375, -31.82812499938547290, 103.1828516163667899 ) ) ;
#4337 = CARTESIAN_POINT ( 'NONE',  ( 235.3564303562499447, -34.45312499938548001, -48.40857419181671162 ) ) ;
#4338 = PLANE ( 'NONE',  #3649 ) ;
#4339 = CARTESIAN_POINT ( 'NONE',  ( 81.02178482187500208, -34.34062499938548285, 102.3871387122750889 ) ) ;
#4340 = CARTESIAN_POINT ( 'NONE',  ( 85.15643035624999868, -30.55312499938548854, -101.5914258081833879 ) ) ;
#4341 = CARTESIAN_POINT ( 'NONE',  ( 235.3564303562499447, -34.45312499938548001, -48.40857419181671162 ) ) ;
#4342 = CARTESIAN_POINT ( 'NONE',  ( -81.59615242270662350, -31.42634618820330772, 97.00000000000000000 ) ) ;
#4343 = CARTESIAN_POINT ( 'NONE',  ( 85.15643035625001289, -33.29062499938547859, -99.99999999999998579 ) ) ;
#4344 = ADVANCED_FACE ( 'NONE', ( #16825 ), #17416, .T. ) ;
#4345 = EDGE_LOOP ( 'NONE', ( #9685, #10871 ) ) ;
#4346 = DIRECTION ( 'NONE',  ( 1.000000000000000000, -0.000000000000000000, -2.407412430484046130E-31 ) ) ;
#4347 = DIRECTION ( 'NONE',  ( 1.000000000000000000, 0.000000000000000000, 0.000000000000000000 ) ) ;
#4348 = CARTESIAN_POINT ( 'NONE',  ( 232.5999999999999375, -30.36562499938548498, -53.18285161636690361 ) ) ;
#4349 = CARTESIAN_POINT ( 'NONE',  ( -81.02178482187500208, -33.89062499938548711, 97.61286128772489690 ) ) ;
#4350 = VERTEX_POINT ( 'NONE', #2163 ) ;
#4351 = CARTESIAN_POINT ( 'NONE',  ( 233.9782151781249411, -32.54062499938547859, 97.61286128772489690 ) ) ;
#4352 = CARTESIAN_POINT ( 'NONE',  ( 82.39999999999999147, -32.98124999877096286, -102.9999999999999858 ) ) ;
#4353 = CARTESIAN_POINT ( 'NONE',  ( -79.39999999999999147, -31.60856250001229029, 101.7320508075688537 ) ) ;
#4354 = ADVANCED_FACE ( 'NONE', ( #8119 ), #18196, .T. ) ;
#4355 = ADVANCED_FACE ( 'NONE', ( #614 ), #12106, .T. ) ;
#4356 = CARTESIAN_POINT ( 'NONE',  ( 82.39999999999999147, -34.33124999877097139, -103.0000000000000000 ) ) ;
#4357 = FACE_OUTER_BOUND ( 'NONE', #7999, .T. ) ;
#4358 = CARTESIAN_POINT ( 'NONE',  ( -81.02178482187500208, -32.24062499938548854, 102.3871387122750889 ) ) ;
#4359 = CARTESIAN_POINT ( 'NONE',  ( -79.39999999999999147, -32.51250000000000284, 101.7320508075688537 ) ) ;
#4360 = CARTESIAN_POINT ( 'NONE',  ( 82.39999999999999147, -32.16562499938549280, 103.1828516163667899 ) ) ;
#4361 = ADVANCED_FACE ( 'NONE', ( #4815 ), #14168, .F. ) ;
#4362 = CARTESIAN_POINT ( 'NONE',  ( -85.40000000000000568, -32.70000000000000284, 99.99999999999998579 ) ) ;
#4363 = CARTESIAN_POINT ( 'NONE',  ( 231.6794753800827777, -34.98323688327302960, 97.06736352196708140 ) ) ;
#4364 = CARTESIAN_POINT ( 'NONE',  ( -82.39999999999999147, -32.16562499938548569, 96.81714838363319586 ) ) ;
#4365 = CARTESIAN_POINT ( 'NONE',  ( -85.15643035624999868, -30.74062499938548143, -101.5914258081833879 ) ) ;
#4366 = ORIENTED_EDGE ( 'NONE', *, *, #1350, .T. ) ;
#4367 = CARTESIAN_POINT ( 'NONE',  ( 85.40000000000000568, -33.13124999877096855, 101.7320508075688679 ) ) ;
#4368 = CARTESIAN_POINT ( 'NONE',  ( 232.5999999999999375, -29.99999999999999645, 99.99999999999998579 ) ) ;
#4369 = CARTESIAN_POINT ( 'NONE',  ( 229.8435696437499871, -35.16562499938547148, -48.40857419181671162 ) ) ;
#4370 = CARTESIAN_POINT ( 'NONE',  ( -82.39999999999999147, -31.94062499938548427, 103.1828516163667899 ) ) ;
#4371 = CYLINDRICAL_SURFACE ( 'NONE', #3993, 2.200000000000007283 ) ;
#4372 = ORIENTED_EDGE ( 'NONE', *, *, #15167, .T. ) ;
#4373 = EDGE_CURVE ( 'NONE', #10751, #7830, #13299, .T. ) ;
#4374 = CARTESIAN_POINT ( 'NONE',  ( -81.02178482187500208, -34.34062499938548285, -102.3871387122750889 ) ) ;
#4375 = CARTESIAN_POINT ( 'NONE',  ( 100.0000000000000000, 10.19999999999997620, -137.3499999999999943 ) ) ;
#4376 = ORIENTED_EDGE ( 'NONE', *, *, #1121, .F. ) ;
#4377 = CARTESIAN_POINT ( 'NONE',  ( -83.20384757729335945, -32.28615380933863577, 97.00000000000000000 ) ) ;
#4378 = CARTESIAN_POINT ( 'NONE',  ( -79.64356964375001269, -32.69062499938548427, -101.5914258081833879 ) ) ;
#4379 = CARTESIAN_POINT ( 'NONE',  ( -79.68063642052034368, -32.00000000000000711, -101.2652131117249752 ) ) ;
#4380 = CARTESIAN_POINT ( 'NONE',  ( -79.39999999999999147, -31.55624999877096926, -98.26794919243113213 ) ) ;
#4381 = CARTESIAN_POINT ( 'NONE',  ( 232.5999999999999375, -31.71562499938547930, 96.81714838363319586 ) ) ;
#4382 = CARTESIAN_POINT ( 'NONE',  ( -83.90000000000000568, -32.12268749875867968, 102.5980762113533018 ) ) ;
#4383 = CARTESIAN_POINT ( 'NONE',  ( -79.64356964375001269, -34.11562499938548854, 101.5914258081833879 ) ) ;
#4384 = CARTESIAN_POINT ( 'NONE',  ( -83.77821517812500929, -34.71562499938548285, -102.3871387122750889 ) ) ;
#4385 = DIRECTION ( 'NONE',  ( -1.000000000000000000, 1.586032892321652482E-15, 0.000000000000000000 ) ) ;
#4386 = FACE_OUTER_BOUND ( 'NONE', #15695, .T. ) ;
#4387 = ADVANCED_FACE ( 'NONE', ( #512 ), #3527, .F. ) ;
#4388 = CARTESIAN_POINT ( 'NONE',  ( 85.40000000000000568, -32.60624999877097707, -101.7320508075688679 ) ) ;
#4389 = CARTESIAN_POINT ( 'NONE',  ( 229.5999999999999375, -32.69999999999999574, 99.99999999999998579 ) ) ;
#4390 = ORIENTED_EDGE ( 'NONE', *, *, #8503, .T. ) ;
#4391 = CARTESIAN_POINT ( 'NONE',  ( 232.5999999999999375, -34.78124999877096002, 102.9999999999999858 ) ) ;
#4392 = CARTESIAN_POINT ( 'NONE',  ( 234.0999999999999375, -34.29374999877096286, 102.5980762113533018 ) ) ;
#4393 = CARTESIAN_POINT ( 'NONE',  ( 229.5999999999999375, -34.03124999877096002, -51.73205080756898866 ) ) ;
#4394 = CARTESIAN_POINT ( 'NONE',  ( -79.64356964374999848, -33.51562499938548711, 99.99999999999998579 ) ) ;
#4395 = ORIENTED_EDGE ( 'NONE', *, *, #5417, .F. ) ;
#4397 = VERTEX_POINT ( 'NONE', #992 ) ;
#4396 = EDGE_CURVE ( 'NONE', #4731, #15882, #16016, .T. ) ;
#4398 = PRODUCT_DEFINITION ( 'UNKNOWN', '', #19243, #3375 ) ;
#4399 = CARTESIAN_POINT ( 'NONE',  ( -79.39999999999999147, -32.06250000000000000, 101.7320508075688537 ) ) ;
#4400 = CYLINDRICAL_SURFACE ( 'NONE', #1630, 6.000000000000015987 ) ;
#4401 = CARTESIAN_POINT ( 'NONE',  ( 4.175813232069148562, 4.122719923832742772, -5.545971589517866732E-16 ) ) ;
#4402 = ORIENTED_EDGE ( 'NONE', *, *, #11313, .T. ) ;
#4403 = DIRECTION ( 'NONE',  ( 0.000000000000000000, 0.000000000000000000, 1.000000000000000000 ) ) ;
#4404 = CARTESIAN_POINT ( 'NONE',  ( 232.5999999999999091, -34.10624999877096286, 96.99999999999998579 ) ) ;
#4405 = CARTESIAN_POINT ( 'NONE',  ( -82.39999999999999147, -33.29062499938549280, 103.1828516163667899 ) ) ;
#4406 = CARTESIAN_POINT ( 'NONE',  ( -82.39999999999999147, -32.58750000000000568, 103.4641016151377499 ) ) ;
#4407 = CARTESIAN_POINT ( 'NONE',  ( -79.39999999999999147, -31.96874999877096712, 99.99999999999998579 ) ) ;
#4408 = CARTESIAN_POINT ( 'NONE',  ( 0.000000000000000000, 3.031088913245533867, 1.750000000000002887 ) ) ;
#4409 = CARTESIAN_POINT ( 'NONE',  ( 80.85389467647095785, -34.99999999999999289, 102.4890844034575395 ) ) ;
#4410 = CARTESIAN_POINT ( 'NONE',  ( -79.59365286754817248, -34.99999999999999289, -100.0710144471396177 ) ) ;
#4411 = FACE_OUTER_BOUND ( 'NONE', #14793, .T. ) ;
#4412 = ORIENTED_EDGE ( 'NONE', *, *, #4702, .F. ) ;
#4413 = PRESENTATION_STYLE_ASSIGNMENT (( #8611 ) ) ;
#4414 = CARTESIAN_POINT ( 'NONE',  ( -79.64356964375001269, -31.22812499938548925, -101.5914258081833879 ) ) ;
#4415 = DIRECTION ( 'NONE',  ( 1.000000000000000000, 0.000000000000000000, 0.000000000000000000 ) ) ;
#4416 = CARTESIAN_POINT ( 'NONE',  ( 82.40000000000000568, -30.00000000000000355, -103.0000000000000000 ) ) ;
#4417 = CARTESIAN_POINT ( 'NONE',  ( 232.5999999999999375, -29.99999999999999645, 103.0000000000000000 ) ) ;
#4418 = CARTESIAN_POINT ( 'NONE',  ( -83.77821517812500929, -30.51562499938548711, 102.3871387122750889 ) ) ;
#4419 = LINE ( 'NONE', #4133, #6938 ) ;
#4420 = CARTESIAN_POINT ( 'NONE',  ( 232.5999999999999375, -33.40312499938547575, -53.18285161636690361 ) ) ;
#4421 = ORIENTED_EDGE ( 'NONE', *, *, #15209, .T. ) ;
#4422 = ORIENTED_EDGE ( 'NONE', *, *, #3031, .F. ) ;
#4423 = CARTESIAN_POINT ( 'NONE',  ( 102.9999999999999858, -29.80000000000000071, -100.0000000000000000 ) ) ;
#4424 = CARTESIAN_POINT ( 'NONE',  ( -79.39999999999999147, -31.08750000000000213, 98.26794919243110371 ) ) ;
#4425 = CARTESIAN_POINT ( 'NONE',  ( -80.90000000000000568, -31.44374999877096855, 97.40192378864668399 ) ) ;
#4426 = CARTESIAN_POINT ( 'NONE',  ( 85.40000000000000568, -33.11250000000000426, 98.26794919243111792 ) ) ;
#4427 = CARTESIAN_POINT ( 'NONE',  ( -79.68596062386970402, -32.00000000000002132, -98.72172371342720965 ) ) ;
#4428 = CARTESIAN_POINT ( 'NONE',  ( 232.5999999999999375, -34.07812499938548001, 103.1828516163667899 ) ) ;
#4429 = CARTESIAN_POINT ( 'NONE',  ( 85.40000000000000568, -32.19374999877096855, 99.99999999999998579 ) ) ;
#4430 = CARTESIAN_POINT ( 'NONE',  ( 83.77821517812500929, -33.66562499938548569, 97.61286128772489690 ) ) ;
#4431 = AXIS2_PLACEMENT_3D ( 'NONE', #4796, #15234, #8197 ) ;
#4432 = CIRCLE ( 'NONE', #15351, 5.199999999999996625 ) ;
#4433 = CARTESIAN_POINT ( 'NONE',  ( 79.64356964375001269, -31.75312499938548427, -101.5914258081833879 ) ) ;
#4434 = EDGE_LOOP ( 'NONE', ( #9114, #12294, #4015, #3573 ) ) ;
#4435 = CARTESIAN_POINT ( 'NONE',  ( 229.8435696437499303, -35.09062499938547575, -50.00000000000011369 ) ) ;
#4436 = CARTESIAN_POINT ( 'NONE',  ( 79.39999999999999147, -34.18124999877097281, 101.7320508075688963 ) ) ;
#4437 = CARTESIAN_POINT ( 'NONE',  ( 83.77821517812500929, -33.66562499938548569, -102.3871387122750889 ) ) ;
#4438 = EDGE_LOOP ( 'NONE', ( #15524, #15428, #18260, #13925 ) ) ;
#4439 = CARTESIAN_POINT ( 'NONE',  ( -82.40000000000000568, -32.00000000000000000, 99.99999999999998579 ) ) ;
#4440 = CARTESIAN_POINT ( 'NONE',  ( 235.5999999999999375, -32.86874999877096570, 99.99999999999998579 ) ) ;
#4441 = CARTESIAN_POINT ( 'NONE',  ( 235.3564303562499447, -31.79062499938547859, -51.59142580818350865 ) ) ;
#4442 = CARTESIAN_POINT ( 'NONE',  ( -85.40000000000000568, -30.00000000000000355, 99.99999999999998579 ) ) ;
#4443 = VERTEX_POINT ( 'NONE', #12994 ) ;
#4444 = DIRECTION ( 'NONE',  ( 0.000000000000000000, 0.000000000000000000, -1.000000000000000000 ) ) ;
#4445 = AXIS2_PLACEMENT_3D ( 'NONE', #1671, #10745, #11831 ) ;
#4446 = VECTOR ( 'NONE', #7580, 1000.000000000000000 ) ;
#4447 = CARTESIAN_POINT ( 'NONE',  ( -80.90000000000000568, -34.20000000000000284, 97.40192378864668399 ) ) ;
#4448 = CARTESIAN_POINT ( 'NONE',  ( 0.000000000000000000, 0.000000000000000000, 0.000000000000000000 ) ) ;
#4449 = CARTESIAN_POINT ( 'NONE',  ( -79.39999999999999147, -32.05856250001228602, 101.7320508075688537 ) ) ;
#4450 = EDGE_CURVE ( 'NONE', #16779, #9677, #18256, .T. ) ;
#4451 = EDGE_CURVE ( 'NONE', #3788, #15137, #5077, .T. ) ;
#4452 = CARTESIAN_POINT ( 'NONE',  ( 1.567478505476134606E-15, 4.618802153517012066, -3.433295621305382905 ) ) ;
#4453 = CARTESIAN_POINT ( 'NONE',  ( -79.39999999999999147, -32.41874999877096997, 99.99999999999998579 ) ) ;
#4454 = CARTESIAN_POINT ( 'NONE',  ( -79.64356964375001269, -31.22812499938548925, 98.40857419181659793 ) ) ;
#4455 = CARTESIAN_POINT ( 'NONE',  ( 81.02178482187500208, -31.90312499938548996, 97.61286128772489690 ) ) ;
#4456 = CARTESIAN_POINT ( 'NONE',  ( -82.39999999999999147, -34.83749999999999858, -97.00000000000000000 ) ) ;
#4457 = CARTESIAN_POINT ( 'NONE',  ( -94.79999999999999716, -29.80000000000000426, 150.0000000000000000 ) ) ;
#4458 = CARTESIAN_POINT ( 'NONE',  ( -84.28136653320150629, -32.00000000000001421, -102.0145392219080378 ) ) ;
#4459 = CARTESIAN_POINT ( 'NONE',  ( -81.02178482187500208, -32.20312499938548711, -102.3871387122750889 ) ) ;
#4460 = CIRCLE ( 'NONE', #16009, 2.500000000000000444 ) ;
#4461 = ORIENTED_EDGE ( 'NONE', *, *, #11966, .T. ) ;
#4462 = CARTESIAN_POINT ( 'NONE',  ( 85.15643035625001289, -31.15312499938548996, 99.99999999999998579 ) ) ;
#4463 = PLANE ( 'NONE',  #3350 ) ;
#4464 = CARTESIAN_POINT ( 'NONE',  ( 82.40000000000001990, -32.53124999877097423, 97.00000000000000000 ) ) ;
#4465 = EDGE_CURVE ( 'NONE', #11020, #7039, #13361, .T. ) ;
#4466 = CARTESIAN_POINT ( 'NONE',  ( -79.64356964375001269, -30.89062499938548711, 98.40857419181659793 ) ) ;
#4467 = CARTESIAN_POINT ( 'NONE',  ( 113.0000000000000000, 10.39615242270649453, -149.9961509411812415 ) ) ;
#4468 = VERTEX_POINT ( 'NONE', #12584 ) ;
#4469 = EDGE_CURVE ( 'NONE', #14259, #13128, #799, .T. ) ;
#4470 = CARTESIAN_POINT ( 'NONE',  ( -81.02178482187500208, -34.04062499938548569, -97.61286128772489690 ) ) ;
#4471 = CARTESIAN_POINT ( 'NONE',  ( 3.961545574370306966, 1.423222908132971476, -3.499999999999999556 ) ) ;
#4472 = CARTESIAN_POINT ( 'NONE',  ( 229.5999999999999375, -33.63749999999999574, -51.73205080756898866 ) ) ;
#4473 = CARTESIAN_POINT ( 'NONE',  ( -79.64356964374999848, -33.17812499938548854, -99.99999999999998579 ) ) ;
#4474 = CARTESIAN_POINT ( 'NONE',  ( -79.58826230849692251, -32.00000000000093792, -101.0460072438472139 ) ) ;
#4475 = CARTESIAN_POINT ( 'NONE',  ( -79.39999999999999147, -31.93124999877096926, -101.7320508075688821 ) ) ;
#4476 = CARTESIAN_POINT ( 'NONE',  ( 235.3564303562499447, -31.82812499938547646, 99.99999999999998579 ) ) ;
#4477 = CARTESIAN_POINT ( 'NONE',  ( -82.39999999999999147, -30.96018749875868181, 96.53589838486223584 ) ) ;
#4478 = CARTESIAN_POINT ( 'NONE',  ( -79.64356964374999848, -34.07812499938548711, 99.99999999999998579 ) ) ;
#4479 = CARTESIAN_POINT ( 'NONE',  ( -81.59615242270660929, -31.48259618943233207, 96.99999999999997158 ) ) ;
#4480 = CARTESIAN_POINT ( 'NONE',  ( 83.77821517812500929, -33.21562499938548285, 97.61286128772489690 ) ) ;
#4481 = CARTESIAN_POINT ( 'NONE',  ( -4.197393957002303999, -0.8151795401431414234, -3.503767560748935139 ) ) ;
#4482 = DIRECTION ( 'NONE',  ( 0.000000000000000000, -0.5000000000000006661, 0.8660254037844382635 ) ) ;
#4483 = CARTESIAN_POINT ( 'NONE',  ( 79.39999999999999147, -34.18124999877097281, -98.26794919243110371 ) ) ;
#4484 = CARTESIAN_POINT ( 'NONE',  ( 231.0999999999999375, -33.07499999999999574, 102.5980762113533018 ) ) ;
#4485 = ORIENTED_EDGE ( 'NONE', *, *, #1639, .T. ) ;
#4486 = CARTESIAN_POINT ( 'NONE',  ( 229.8435696437499303, -33.40312499938547575, -50.00000000000011369 ) ) ;
#4487 = DIRECTION ( 'NONE',  ( -1.000000000000000000, -1.336382355046098552E-47, 4.814824860968092260E-31 ) ) ;
#4488 = CARTESIAN_POINT ( 'NONE',  ( 232.5999999999999375, -35.00624999877096855, 96.53589838486223584 ) ) ;
#4489 = CARTESIAN_POINT ( 'NONE',  ( 232.5999999999999375, -32.53124999877096002, -46.53589838486234953 ) ) ;
#4490 = CARTESIAN_POINT ( 'NONE',  ( -85.15643035625001289, -34.60312499938548569, 101.5914258081833879 ) ) ;
#4491 = VERTEX_POINT ( 'NONE', #18456 ) ;
#4492 = VERTEX_POINT ( 'NONE', #4883 ) ;
#4493 = CARTESIAN_POINT ( 'NONE',  ( 25.15499999999999758, 0.000000000000000000, 0.000000000000000000 ) ) ;
#4494 = CARTESIAN_POINT ( 'NONE',  ( -84.70833260042415702, -35.00006955123599539, 98.08383195543535749 ) ) ;
#4495 = CARTESIAN_POINT ( 'NONE',  ( 4.175813232069151226, -4.122719923832748101, -3.898053888241413974E-16 ) ) ;
#4496 = ORIENTED_EDGE ( 'NONE', *, *, #10471, .F. ) ;
#4497 = CARTESIAN_POINT ( 'NONE',  ( 80.90000000000000568, -32.34374999877096712, -97.40192378864668399 ) ) ;
#4498 = LINE ( 'NONE', #18176, #5818 ) ;
#4499 = SHAPE_REPRESENTATION ( 'tray', ( #10540 ), #13638 ) ;
#4500 = CARTESIAN_POINT ( 'NONE',  ( -82.39999999999999147, -35.09062499938548285, 103.1828516163667899 ) ) ;
#4501 = CARTESIAN_POINT ( 'NONE',  ( -82.39999999999999147, -34.38750000000000284, 103.4641016151377499 ) ) ;
#4502 = CARTESIAN_POINT ( 'NONE',  ( -85.40000000000000568, -30.80624999877096926, 101.7320508075688679 ) ) ;
#4503 = DIRECTION ( 'NONE',  ( -0.000000000000000000, 1.000000000000000000, -0.000000000000000000 ) ) ;
#4504 = EDGE_CURVE ( 'NONE', #12559, #15718, #8882, .T. ) ;
#4505 = DIRECTION ( 'NONE',  ( 0.000000000000000000, -1.000000000000000000, 0.000000000000000000 ) ) ;
#4506 = CARTESIAN_POINT ( 'NONE',  ( 82.39999999999999147, -33.65624999877097423, 103.0000000000000000 ) ) ;
#4507 = CARTESIAN_POINT ( 'NONE',  ( -82.40000000000000568, -34.55624999877097281, -102.9999999999999858 ) ) ;
#4508 = ORIENTED_EDGE ( 'NONE', *, *, #13701, .T. ) ;
#4509 = CARTESIAN_POINT ( 'NONE',  ( -83.77821517812500929, -33.21562499938548285, -97.61286128772489690 ) ) ;
#4510 = CARTESIAN_POINT ( 'NONE',  ( 4.175002511812151873, 2.208363329454889445, -3.469254087858244073 ) ) ;
#4511 = CARTESIAN_POINT ( 'NONE',  ( 0.000000000000000000, 0.000000000000000000, 0.000000000000000000 ) ) ;
#4512 = CARTESIAN_POINT ( 'NONE',  ( 80.52691934816498076, -34.99999999999999289, -102.0537355158132868 ) ) ;
#4513 = CARTESIAN_POINT ( 'NONE',  ( -79.64356964375001269, -30.32812499938548711, 98.40857419181659793 ) ) ;
#4514 = CARTESIAN_POINT ( 'NONE',  ( 232.5999999999999375, -32.27812499938547575, -46.81714838363331666 ) ) ;
#4515 = PRODUCT_RELATED_PRODUCT_CATEGORY ( 'part', '', ( #12793 ) ) ;
#4516 = VERTEX_POINT ( 'NONE', #16894 ) ;
#4517 = ORIENTED_EDGE ( 'NONE', *, *, #4373, .T. ) ;
#4518 = CARTESIAN_POINT ( 'NONE',  ( -80.90000000000000568, -34.80000000000000426, -97.40192378864668399 ) ) ;
#4519 = CARTESIAN_POINT ( 'NONE',  ( -82.39999999999999147, -30.33750000000000213, 103.4641016151377499 ) ) ;
#4520 = CARTESIAN_POINT ( 'NONE',  ( -83.90000000000000568, -32.71874999877096712, 97.40192378864668399 ) ) ;
#4521 = CARTESIAN_POINT ( 'NONE',  ( 80.90000000000000568, -31.05000000000000071, 102.5980762113533018 ) ) ;
#4522 = EDGE_CURVE ( 'NONE', #3020, #5869, #5402, .T. ) ;
#4523 = CARTESIAN_POINT ( 'NONE',  ( -4.000000000000000000, 2.309401076758498483, -3.433295621305379353 ) ) ;
#4524 = CARTESIAN_POINT ( 'NONE',  ( 229.8435696437499871, -34.22812499938547148, 98.40857419181659793 ) ) ;
#4525 = B_SPLINE_CURVE_WITH_KNOTS ( 'NONE', 3,
 ( #18197, #333, #6281, #15061, #228, #3232, #13784, #12134, #10660, #513, #15256, #9192, #13691, #18389, #5009, #12225, #426, #1590 ),
 .UNSPECIFIED., .F., .F.,
 ( 4, 2, 2, 2, 2, 2, 2, 2, 4 ),
 ( 0.000000000000000000, 0.0007089252359836048425, 0.001417850471967209685, 0.002126775707950814311, 0.002835700943934419370, 0.003544626179918024429, 0.004253551415901628621, 0.004962476651885233681, 0.005671401887868838740 ),
 .UNSPECIFIED. ) ;
#4526 = CARTESIAN_POINT ( 'NONE',  ( 235.3564303562499447, -33.47812499938547859, -51.59142580818350154 ) ) ;
#4527 = CARTESIAN_POINT ( 'NONE',  ( 79.64356964375001269, -34.82812499938548711, 101.5914258081833879 ) ) ;
#4528 = VECTOR ( 'NONE', #14030, 1000.000000000000000 ) ;
#4529 = CARTESIAN_POINT ( 'NONE',  ( 83.77821517812500929, -32.31562499938548427, -102.3871387122750889 ) ) ;
#4530 = ORIENTED_EDGE ( 'NONE', *, *, #8590, .T. ) ;
#4531 = CARTESIAN_POINT ( 'NONE',  ( 234.0999999999999375, -30.74999999999999645, -47.40192378864679768 ) ) ;
#4532 = CARTESIAN_POINT ( 'NONE',  ( -81.02178482187500208, -34.79062499938548569, 97.61286128772489690 ) ) ;
#4533 = CARTESIAN_POINT ( 'NONE',  ( 85.15643035624999868, -33.32812499938548001, -98.40857419181659793 ) ) ;
#4534 = DIRECTION ( 'NONE',  ( 0.000000000000000000, -1.000000000000000000, 0.000000000000000000 ) ) ;
#4535 = DIRECTION ( 'NONE',  ( -1.000000000000000000, 0.000000000000000000, 0.000000000000000000 ) ) ;
#4536 = CARTESIAN_POINT ( 'NONE',  ( 231.2217848218749339, -31.07812499938548001, -47.61286128772501769 ) ) ;
#4537 = CARTESIAN_POINT ( 'NONE',  ( -82.39999999999999147, -34.52812499938548996, 103.1828516163667899 ) ) ;
#4538 = ORIENTED_EDGE ( 'NONE', *, *, #8760, .F. ) ;
#4539 = DIRECTION ( 'NONE',  ( -0.000000000000000000, -1.000000000000000000, -0.000000000000000000 ) ) ;
#4540 = EDGE_CURVE ( 'NONE', #9588, #10258, #7399, .T. ) ;
#4541 = EDGE_CURVE ( 'NONE', #7039, #11136, #12486, .T. ) ;
#4542 = CIRCLE ( 'NONE', #10784, 2.649999999999980371 ) ;
#4543 = CARTESIAN_POINT ( 'NONE',  ( 233.9782151781249411, -33.89062499938548001, 97.61286128772489690 ) ) ;
#4544 = CARTESIAN_POINT ( 'NONE',  ( -82.40000000000000568, -30.00000000000000355, 96.99999999999998579 ) ) ;
#4545 =( BOUNDED_CURVE ( )  B_SPLINE_CURVE ( 2, ( #15953, #2556, #8519, #1101, #17710, #10659, #16535 ),
 .UNSPECIFIED., .F., .F. ) 
 B_SPLINE_CURVE_WITH_KNOTS ( ( 3, 2, 2, 3 ),
 ( 0.8958333333333333703, 0.9027777777777777901, 0.9166666666666666297, 0.9258785066912882389 ),
 .UNSPECIFIED. ) 
 CURVE ( )  GEOMETRIC_REPRESENTATION_ITEM ( )  RATIONAL_B_SPLINE_CURVE ( ( 0.9330127018922192983, 0.9330127018922198534, 1.000000000000000000, 0.8660254037844387076, 1.000000000000000000, 0.9111410165655264848, 0.9401539157124900736 ) ) 
 REPRESENTATION_ITEM ( '' )  );
#4546 = CARTESIAN_POINT ( 'NONE',  ( -80.90000000000000568, -31.64606250001229881, 102.5980762113533018 ) ) ;
#4547 = CARTESIAN_POINT ( 'NONE',  ( -82.39999999999999147, -32.58749999999999858, -96.99999999999998579 ) ) ;
#4548 = CARTESIAN_POINT ( 'NONE',  ( -83.90000000000000568, -32.17500000000000426, 102.5980762113533018 ) ) ;
#4549 = CARTESIAN_POINT ( 'NONE',  ( -85.15643035624999868, -32.42812499938548854, 98.40857419181659793 ) ) ;
#4550 = CARTESIAN_POINT ( 'NONE',  ( 82.39999999999999147, -31.94062499938548427, 96.81714838363319586 ) ) ;
#4551 = CARTESIAN_POINT ( 'NONE',  ( 81.02178482187500208, -30.40312499938548640, -97.61286128772489690 ) ) ;
#4552 = DIRECTION ( 'NONE',  ( 0.000000000000000000, 1.000000000000000000, 0.000000000000000000 ) ) ;
#4553 = LINE ( 'NONE', #10608, #4446 ) ;
#4554 = CARTESIAN_POINT ( 'NONE',  ( -81.02178482187500208, -31.75312499938548427, -102.3871387122750889 ) ) ;
#4555 = AXIS2_PLACEMENT_3D ( 'NONE', #1974, #15457, #12428 ) ;
#4556 = VERTEX_POINT ( 'NONE', #5167 ) ;
#4557 = CARTESIAN_POINT ( 'NONE',  ( 79.64356964375001269, -30.89062499938548711, 101.5914258081833879 ) ) ;
#4558 = FACE_OUTER_BOUND ( 'NONE', #7055, .T. ) ;
#4559 = DIRECTION ( 'NONE',  ( -1.000000000000000000, 0.000000000000000000, 0.000000000000000000 ) ) ;
#4560 = CARTESIAN_POINT ( 'NONE',  ( -82.40000000000000568, -33.03750000000000142, 102.9999999999999858 ) ) ;
#4561 = CARTESIAN_POINT ( 'NONE',  ( -85.15643035624999868, -32.46562499938548996, 101.5914258081833879 ) ) ;
#4562 = CYLINDRICAL_SURFACE ( 'NONE', #7744, 3.000000000000009770 ) ;
#4563 = ORIENTED_EDGE ( 'NONE', *, *, #3925, .T. ) ;
#4564 = CARTESIAN_POINT ( 'NONE',  ( -85.40000000000000568, -31.76249999999999929, -98.26794919243111792 ) ) ;
#4565 = CARTESIAN_POINT ( 'NONE',  ( 4.204115023516791005, -1.660442669500199919, -3.602151381774560068 ) ) ;
#4566 = CARTESIAN_POINT ( 'NONE',  ( 80.90000000000000568, -33.69374999877096855, 102.5980762113533018 ) ) ;
#4567 = CARTESIAN_POINT ( 'NONE',  ( -81.02178482187500208, -33.55312499938548854, -102.3871387122750889 ) ) ;
#4568 = VECTOR ( 'NONE', #14819, 1000.000000000000000 ) ;
#4569 = LINE ( 'NONE', #9056, #17996 ) ;
#4570 = CARTESIAN_POINT ( 'NONE',  ( 233.9782151781249411, -32.20312499938548001, 97.61286128772489690 ) ) ;
#4571 = CARTESIAN_POINT ( 'NONE',  ( -85.40000000000000568, -32.68518749875868679, 98.26794919243111792 ) ) ;
#4572 = CARTESIAN_POINT ( 'NONE',  ( -85.15643035624999868, -32.99062499938548854, 98.40857419181659793 ) ) ;
#4573 = CARTESIAN_POINT ( 'NONE',  ( -85.15643035625001289, -34.64062499938548711, -99.99999999999998579 ) ) ;
#4574 = CARTESIAN_POINT ( 'NONE',  ( 79.64356964374999848, -33.96562499938548285, 99.99999999999998579 ) ) ;
#4575 = DIRECTION ( 'NONE',  ( 0.000000000000000000, 0.000000000000000000, 1.000000000000000000 ) ) ;
#4576 = EDGE_CURVE ( 'NONE', #5794, #6376, #4790, .T. ) ;
#4577 = EDGE_CURVE ( 'NONE', #104, #3780, #18687, .T. ) ;
#4578 =( BOUNDED_CURVE ( )  B_SPLINE_CURVE ( 2, ( #8749, #11780, #2692, #13239, #14608, #8649, #17650, #11398, #10128 ),
 .UNSPECIFIED., .F., .F. ) 
 B_SPLINE_CURVE_WITH_KNOTS ( ( 3, 2, 2, 2, 3 ),
 ( 0.3958333333333334259, 0.4027777777777777901, 0.4166666666666666852, 0.4305555555555555802, 0.4374999999999999445 ),
 .UNSPECIFIED. ) 
 CURVE ( )  GEOMETRIC_REPRESENTATION_ITEM ( )  RATIONAL_B_SPLINE_CURVE ( ( 0.9330127018922192983, 0.9330127018922200755, 1.000000000000000000, 0.8660254037844387076, 1.000000000000000000, 0.8660254037844387076, 1.000000000000000000, 0.9330127018922198534, 0.9330127018922192983 ) ) 
 REPRESENTATION_ITEM ( '' )  );
#4579 = CARTESIAN_POINT ( 'NONE',  ( -82.40000000000000568, -30.11250000000000071, 96.99999999999998579 ) ) ;
#4580 = CARTESIAN_POINT ( 'NONE',  ( 79.39999999999999147, -34.25624999877096855, -101.7320508075688537 ) ) ;
#4581 = CARTESIAN_POINT ( 'NONE',  ( 235.5999999999999943, -34.68749999999999289, 98.26794919243110371 ) ) ;
#4582 = ORIENTED_EDGE ( 'NONE', *, *, #15340, .T. ) ;
#4583 = CARTESIAN_POINT ( 'NONE',  ( 232.5999999999999943, -33.29062499938547859, -46.81714838363331666 ) ) ;
#4584 = DIRECTION ( 'NONE',  ( 1.000000000000000000, 0.000000000000000000, 0.000000000000000000 ) ) ;
#4585 = CARTESIAN_POINT ( 'NONE',  ( 231.2217848218749339, -31.07812499938548001, 102.3871387122750889 ) ) ;
#4586 = CARTESIAN_POINT ( 'NONE',  ( 232.5999999999999375, -33.65624999877096002, -53.46410161513786363 ) ) ;
#4587 = VECTOR ( 'NONE', #16475, 1000.000000000000000 ) ;
#4588 = ADVANCED_FACE ( 'NONE', ( #8469 ), #11316, .F. ) ;
#4589 = CARTESIAN_POINT ( 'NONE',  ( -82.39999999999999147, -32.72812499938548569, 103.1828516163667899 ) ) ;
#4590 = ORIENTED_EDGE ( 'NONE', *, *, #6653, .F. ) ;
#4591 = ORIENTED_EDGE ( 'NONE', *, *, #15939, .T. ) ;
#4592 = CARTESIAN_POINT ( 'NONE',  ( 4.124214193018032049, 2.028338413290970976, -3.513185186763606804 ) ) ;
#4593 = DIRECTION ( 'NONE',  ( 1.000000000000000000, -1.387778780781445676E-15, -2.407412430484046130E-31 ) ) ;
#4594 = CARTESIAN_POINT ( 'NONE',  ( -85.40000000000000568, -33.63750000000000284, -101.7320508075688821 ) ) ;
#4595 = VERTEX_POINT ( 'NONE', #9851 ) ;
#4596 = CARTESIAN_POINT ( 'NONE',  ( 1.567478505476134606E-15, 4.618802153517012066, -5.000000000000000000 ) ) ;
#4597 = VECTOR ( 'NONE', #2853, 1000.000000000000000 ) ;
#4598 = CARTESIAN_POINT ( 'NONE',  ( 235.5999999999999943, -32.43749999999999289, 98.26794919243110371 ) ) ;
#4599 = CARTESIAN_POINT ( 'NONE',  ( -82.39999999999999147, -34.64062499938548711, 103.1828516163667899 ) ) ;
#4600 = CARTESIAN_POINT ( 'NONE',  ( -85.40000000000000568, -34.91250000000000142, 101.7320508075688679 ) ) ;
#4601 = EDGE_CURVE ( 'NONE', #16690, #10239, #10767, .T. ) ;
#4602 = CARTESIAN_POINT ( 'NONE',  ( -83.90000000000000568, -32.26874999877097139, 97.40192378864668399 ) ) ;
#4603 = DIRECTION ( 'NONE',  ( 0.000000000000000000, 0.000000000000000000, 1.000000000000000000 ) ) ;
#4604 = ADVANCED_FACE ( 'NONE', ( #5656 ), #777, .F. ) ;
#4605 = CARTESIAN_POINT ( 'NONE',  ( 80.90000000000000568, -34.80000000000000426, -102.5980762113533018 ) ) ;
#4606 = CARTESIAN_POINT ( 'NONE',  ( 4.033901012036126943, 2.321269032827665058, 2.979444097106977107 ) ) ;
#4607 = DIRECTION ( 'NONE',  ( 0.000000000000000000, 0.000000000000000000, -1.000000000000000000 ) ) ;
#4608 = ADVANCED_FACE ( 'NONE', ( #874 ), #11480, .F. ) ;
#4609 = CARTESIAN_POINT ( 'NONE',  ( 235.3564303562499447, -31.30312499938547788, 101.5914258081833879 ) ) ;
#4610 = ORIENTED_EDGE ( 'NONE', *, *, #413, .T. ) ;
#4611 = AXIS2_PLACEMENT_3D ( 'NONE', #16049, #2652, #9900 ) ;
#4612 = CARTESIAN_POINT ( 'NONE',  ( -79.64356964375001269, -32.20312499938548001, -98.40857419181659793 ) ) ;
#4613 = CARTESIAN_POINT ( 'NONE',  ( 2.756197834950227410, 3.027510591568626896, -3.223146290109805356 ) ) ;
#4614 = CARTESIAN_POINT ( 'NONE',  ( 234.0999999999999375, -33.74999999999999289, 97.40192378864668399 ) ) ;
#4615 = CARTESIAN_POINT ( 'NONE',  ( 3.973110223765528026, -0.6902454861566470479, 3.565797985667392034 ) ) ;
#4616 = CARTESIAN_POINT ( 'NONE',  ( -83.77821517812500929, -30.96562499938548640, 102.3871387122750889 ) ) ;
#4617 = CARTESIAN_POINT ( 'NONE',  ( 83.90000000000000568, -33.07500000000000284, -102.5980762113533018 ) ) ;
#4618 = CARTESIAN_POINT ( 'NONE',  ( 231.2217848218749339, -35.01562499938548001, -47.61286128772501769 ) ) ;
#4619 = AXIS2_PLACEMENT_3D ( 'NONE', #14912, #1541, #14709 ) ;
#4620 =( BOUNDED_CURVE ( )  B_SPLINE_CURVE ( 2, ( #8684, #5758, #14535, #8778, #13079, #3899, #5383, #2438, #4290 ),
 .UNSPECIFIED., .F., .F. ) 
 B_SPLINE_CURVE_WITH_KNOTS ( ( 3, 2, 2, 2, 3 ),
 ( 0.3958333333333333148, 0.4027777777777777901, 0.4166666666666666852, 0.4305555555555555802, 0.4374999999999999445 ),
 .UNSPECIFIED. ) 
 CURVE ( )  GEOMETRIC_REPRESENTATION_ITEM ( )  RATIONAL_B_SPLINE_CURVE ( ( 0.9330127018922194093, 0.9330127018922190762, 1.000000000000000000, 0.8660254037844387076, 1.000000000000000000, 0.8660254037844387076, 1.000000000000000000, 0.9330127018922198534, 0.9330127018922192983 ) ) 
 REPRESENTATION_ITEM ( '' )  );
#4621 = VERTEX_POINT ( 'NONE', #6837 ) ;
#4622 = ORIENTED_EDGE ( 'NONE', *, *, #15566, .F. ) ;
#4623 = CARTESIAN_POINT ( 'NONE',  ( -82.39999999999999147, -31.91249999999999787, 96.99999999999998579 ) ) ;
#4624 = EDGE_CURVE ( 'NONE', #5649, #1717, #3986, .T. ) ;
#4625 = CARTESIAN_POINT ( 'NONE',  ( -85.40000000000000568, -30.00000000000000355, 99.99999999999998579 ) ) ;
#4626 = CARTESIAN_POINT ( 'NONE',  ( -79.39999999999999147, -31.10624999877097352, 101.7320508075688537 ) ) ;
#4627 = CARTESIAN_POINT ( 'NONE',  ( 85.40000000000000568, -32.28750000000000142, 101.7320508075688679 ) ) ;
#4628 = VECTOR ( 'NONE', #2206, 1000.000000000000000 ) ;
#4629 = DIRECTION ( 'NONE',  ( -0.000000000000000000, -0.000000000000000000, -1.000000000000000000 ) ) ;
#4630 = CARTESIAN_POINT ( 'NONE',  ( 232.5999999999999375, -33.62812499938547717, 103.1828516163667899 ) ) ;
#4631 = CARTESIAN_POINT ( 'NONE',  ( 233.9782151781249411, -33.14062499938548001, -47.61286128772501769 ) ) ;
#4632 = CIRCLE ( 'NONE', #13686, 5.384454397937118664 ) ;
#4633 = CYLINDRICAL_SURFACE ( 'NONE', #10867, 3.000000000000002665 ) ;
#4634 = VECTOR ( 'NONE', #4629, 1000.000000000000000 ) ;
#4635 = B_SPLINE_CURVE_WITH_KNOTS ( 'NONE', 3,
 ( #11997, #7215, #4481, #5856 ),
 .UNSPECIFIED., .F., .F.,
 ( 4, 4 ),
 ( 0.000000000000000000, 0.002452478801916376308 ),
 .UNSPECIFIED. ) ;
#4636 = CARTESIAN_POINT ( 'NONE',  ( 79.64356964375001269, -30.85312499938548569, -101.5914258081833879 ) ) ;
#4637 = ORIENTED_EDGE ( 'NONE', *, *, #1257, .F. ) ;
#4638 = CARTESIAN_POINT ( 'NONE',  ( 234.0999999999999375, -33.29999999999999716, -52.59807621135342970 ) ) ;
#4639 = ADVANCED_FACE ( 'NONE', ( #18652 ), #15907, .F. ) ;
#4640 = CARTESIAN_POINT ( 'NONE',  ( -85.15643035625001289, -34.60312499938548569, 101.5914258081833879 ) ) ;
#4641 = CARTESIAN_POINT ( 'NONE',  ( 81.02178482187500208, -33.59062499938548285, -102.3871387122750889 ) ) ;
#4642 = DIRECTION ( 'NONE',  ( -0.000000000000000000, -1.000000000000000000, -0.000000000000000000 ) ) ;
#4643 = CARTESIAN_POINT ( 'NONE',  ( 105.1999999999999744, -29.80000000000000071, -100.0000000000000000 ) ) ;
#4644 = CARTESIAN_POINT ( 'NONE',  ( 229.8435696437499871, -31.19062499938548072, -51.59142580818350865 ) ) ;
#4645 = CARTESIAN_POINT ( 'NONE',  ( -79.64356964375001269, -34.90312499938548285, 101.5914258081833879 ) ) ;
#4646 = ORIENTED_EDGE ( 'NONE', *, *, #13701, .F. ) ;
#4647 = CARTESIAN_POINT ( 'NONE',  ( 82.39999999999999147, -32.36250000000000426, 102.9999999999999858 ) ) ;
#4648 = VECTOR ( 'NONE', #17272, 1000.000000000000000 ) ;
#4649 = CARTESIAN_POINT ( 'NONE',  ( 232.5999999999999943, -34.52812499938547575, 103.1828516163667899 ) ) ;
#4650 = CARTESIAN_POINT ( 'NONE',  ( 82.39999999999999147, -30.92812499938548143, 96.81714838363319586 ) ) ;
#4651 = CARTESIAN_POINT ( 'NONE',  ( -85.40000000000000568, -33.14606250001229171, 99.99999999999998579 ) ) ;
#4652 = CARTESIAN_POINT ( 'NONE',  ( 2.100000000000000089, 0.000000000000000000, -5.000000000000000000 ) ) ;
#4653 = DIRECTION ( 'NONE',  ( 0.000000000000000000, 0.000000000000000000, -1.000000000000000000 ) ) ;
#4654 = CARTESIAN_POINT ( 'NONE',  ( 235.4117376914898045, -31.99999999999999289, 98.95399275611721635 ) ) ;
#4655 = CARTESIAN_POINT ( 'NONE',  ( 79.64356964375001269, -34.11562499938548854, 98.40857419181659793 ) ) ;
#4656 = CARTESIAN_POINT ( 'NONE',  ( 79.64356964374999848, -30.47812499938548569, -99.99999999999998579 ) ) ;
#4657 = CARTESIAN_POINT ( 'NONE',  ( 232.5999999999999375, -34.78124999877096002, 102.9999999999999858 ) ) ;
#4658 = CARTESIAN_POINT ( 'NONE',  ( -82.40000000000000568, -30.00000000000000355, 96.99999999999998579 ) ) ;
#4659 = CARTESIAN_POINT ( 'NONE',  ( -82.39999999999999147, -31.94062499938548427, -96.81714838363319586 ) ) ;
#4660 = ORIENTED_EDGE ( 'NONE', *, *, #6043, .F. ) ;
#4661 = CARTESIAN_POINT ( 'NONE',  ( 82.39999999999999147, -30.81562499938548427, 103.1828516163667899 ) ) ;
#4662 = CARTESIAN_POINT ( 'NONE',  ( -83.20395887649198130, -35.00000000000002132, 102.6365808225363025 ) ) ;
#4663 = CARTESIAN_POINT ( 'NONE',  ( 244.7999999999999545, -4.999999999999990230, -100.0000000000000995 ) ) ;
#4664 = CARTESIAN_POINT ( 'NONE',  ( -83.77821517812500929, -32.57812499938548711, 97.61286128772489690 ) ) ;
#4665 =( BOUNDED_CURVE ( )  B_SPLINE_CURVE ( 2, ( #11953, #4342, #13223, #6204, #14786, #9025, #245, #12152, #14985 ),
 .UNSPECIFIED., .F., .F. ) 
 B_SPLINE_CURVE_WITH_KNOTS ( ( 3, 2, 2, 2, 3 ),
 ( 0.1875000000000000278, 0.1944444444444444475, 0.2083333333333333426, 0.2222222222222222099, 0.2291666666666666574 ),
 .UNSPECIFIED. ) 
 CURVE ( )  GEOMETRIC_REPRESENTATION_ITEM ( )  RATIONAL_B_SPLINE_CURVE ( ( 0.9330127018922194093, 0.9330127018922196314, 1.000000000000000000, 0.8660254037844387076, 1.000000000000000000, 0.8660254037844387076, 1.000000000000000000, 0.9330127018922194093, 0.9330127018922194093 ) ) 
 REPRESENTATION_ITEM ( '' )  );
#4666 = CARTESIAN_POINT ( 'NONE',  ( 85.40000000000000568, -33.05624999877097281, 98.26794919243111792 ) ) ;
#4667 = EDGE_LOOP ( 'NONE', ( #5538, #3499, #17491, #1307 ) ) ;
#4668 = CARTESIAN_POINT ( 'NONE',  ( -85.40000000000000568, -32.25000000000000000, -99.99999999999998579 ) ) ;
#4669 = CARTESIAN_POINT ( 'NONE',  ( 83.90000000000000568, -34.42500000000000426, -102.5980762113533018 ) ) ;
#4670 = CARTESIAN_POINT ( 'NONE',  ( 83.32052461991715120, -34.98323688327303671, -97.06736352196708140 ) ) ;
#4671 = CARTESIAN_POINT ( 'NONE',  ( -82.39999999999999147, -32.84062499938548996, -96.81714838363319586 ) ) ;
#4672 = CARTESIAN_POINT ( 'NONE',  ( 232.5999999999999375, -29.99999999999999645, 99.99999999999998579 ) ) ;
#4673 = CARTESIAN_POINT ( 'NONE',  ( 232.5999999999999375, -31.04062499938547859, 103.1828516163667899 ) ) ;
#4674 = CARTESIAN_POINT ( 'NONE',  ( -79.39999999999999147, -31.07268749875867897, 99.99999999999998579 ) ) ;
#4675 = CARTESIAN_POINT ( 'NONE',  ( -83.77821517812500929, -34.37812499938548427, 97.61286128772489690 ) ) ;
#4676 = CARTESIAN_POINT ( 'NONE',  ( -82.40000000000000568, -30.00000000000000355, -99.99999999999998579 ) ) ;
#4677 = CARTESIAN_POINT ( 'NONE',  ( 85.15643035625001289, -33.29062499938547859, 99.99999999999998579 ) ) ;
#4678 = FACE_OUTER_BOUND ( 'NONE', #15835, .T. ) ;
#4679 = CYLINDRICAL_SURFACE ( 'NONE', #15186, 3.000000000000002665 ) ;
#4680 = CARTESIAN_POINT ( 'NONE',  ( 83.90000000000000568, -33.01874999877097139, -102.5980762113533018 ) ) ;
#4681 = CARTESIAN_POINT ( 'NONE',  ( 232.5999999999999375, -32.58749999999999858, 103.4641016151377499 ) ) ;
#4682 = ORIENTED_EDGE ( 'NONE', *, *, #19070, .T. ) ;
#4683 = CARTESIAN_POINT ( 'NONE',  ( 233.9782151781249411, -33.55312499938548143, -52.38713871227520968 ) ) ;
#4684 = CARTESIAN_POINT ( 'NONE',  ( 232.5999999999999375, -30.59062499938547930, 103.1828516163667899 ) ) ;
#4685 = CARTESIAN_POINT ( 'NONE',  ( 235.3564303562499447, -31.34062499938548285, -51.59142580818350865 ) ) ;
#4686 = CARTESIAN_POINT ( 'NONE',  ( -85.15643035625001289, -33.74062499938548854, 99.99999999999998579 ) ) ;
#4687 = ORIENTED_EDGE ( 'NONE', *, *, #17240, .F. ) ;
#4688 = EDGE_LOOP ( 'NONE', ( #76, #7655, #11795, #13407 ) ) ;
#4689 = CARTESIAN_POINT ( 'NONE',  ( 232.5999999999999091, -34.38749999999999574, -47.00000000000011369 ) ) ;
#4690 = CARTESIAN_POINT ( 'NONE',  ( -4.000000000000000000, 1.700094919196744270, -3.320312364301766017 ) ) ;
#4691 = LINE ( 'NONE', #18270, #14102 ) ;
#4692 = EDGE_LOOP ( 'NONE', ( #10858, #18154, #4366, #2104 ) ) ;
#4693 = DIRECTION ( 'NONE',  ( 0.000000000000000000, -1.000000000000000000, 0.000000000000000000 ) ) ;
#4694 = CARTESIAN_POINT ( 'NONE',  ( 229.5999999999999375, -33.95624999877096428, 101.7320508075688821 ) ) ;
#4695 = ADVANCED_FACE ( 'NONE', ( #2607 ), #7435, .T. ) ;
#4696 = CARTESIAN_POINT ( 'NONE',  ( -83.77821517812500929, -33.92812499938548854, 97.61286128772489690 ) ) ;
#4697 = CARTESIAN_POINT ( 'NONE',  ( -85.40000000000000568, -33.56250000000000000, 101.7320508075688679 ) ) ;
#4698 =( BOUNDED_CURVE ( )  B_SPLINE_CURVE ( 2, ( #4654, #362, #15095, #7381, #16279, #13341, #18132 ),
 .UNSPECIFIED., .F., .F. ) 
 B_SPLINE_CURVE_WITH_KNOTS ( ( 3, 2, 2, 3 ),
 ( 0.3702305174531553833, 0.3750000000000000000, 0.3888888888888888951, 0.3958333333333333148 ),
 .UNSPECIFIED. ) 
 CURVE ( )  GEOMETRIC_REPRESENTATION_ITEM ( )  RATIONAL_B_SPLINE_CURVE ( ( 0.9395835397632974484, 0.9539927561173113801, 1.000000000000000000, 0.8660254037844387076, 1.000000000000000000, 0.9330127018922196314, 0.9330127018922194093 ) ) 
 REPRESENTATION_ITEM ( '' )  );
#4699 = CARTESIAN_POINT ( 'NONE',  ( -85.40000000000000568, -31.70624999877096784, 101.7320508075688679 ) ) ;
#4700 = DIRECTION ( 'NONE',  ( 0.5000000000000022204, 0.8660254037844374864, -0.000000000000000000 ) ) ;
#4701 = EDGE_CURVE ( 'NONE', #12847, #10833, #171, .T. ) ;
#4702 = EDGE_CURVE ( 'NONE', #15327, #2447, #2369, .T. ) ;
#4703 = CARTESIAN_POINT ( 'NONE',  ( 232.5999999999999375, -32.30624999877096570, -53.00000000000011369 ) ) ;
#4704 = CARTESIAN_POINT ( 'NONE',  ( 235.5999999999999375, -33.37499999999999289, 99.99999999999998579 ) ) ;
#4705 = CARTESIAN_POINT ( 'NONE',  ( -82.40000000000001990, -33.26250000000000284, 97.00000000000000000 ) ) ;
#4706 = CARTESIAN_POINT ( 'NONE',  ( 4.000000000000000000, -1.560351142792952617, -0.2242961665059816367 ) ) ;
#4707 = CARTESIAN_POINT ( 'NONE',  ( 235.3564303562499447, -31.22812499938548214, 98.40857419181659793 ) ) ;
#4708 = ORIENTED_EDGE ( 'NONE', *, *, #7742, .F. ) ;
#4709 = APPLICATION_CONTEXT ( 'automotive_design' ) ;
#4710 =( NAMED_UNIT ( * ) SI_UNIT ( $, .STERADIAN. ) SOLID_ANGLE_UNIT ( ) );
#4711 = CARTESIAN_POINT ( 'NONE',  ( -82.39999999999999147, -32.27812499938548285, -96.81714838363319586 ) ) ;
#4712 = CARTESIAN_POINT ( 'NONE',  ( -0.02511973781850462134, 4.877415612947412882, -3.751298745799839462 ) ) ;
#4713 = PLANE ( 'NONE',  #11139 ) ;
#4714 = CARTESIAN_POINT ( 'NONE',  ( -82.40000000000001990, -32.53124999877097423, 103.0000000000000000 ) ) ;
#4715 = FACE_OUTER_BOUND ( 'NONE', #16745, .T. ) ;
#4716 = CARTESIAN_POINT ( 'NONE',  ( 235.3564303562499447, -34.82812499938548001, -51.59142580818350865 ) ) ;
#4718 = ADVANCED_FACE ( 'NONE', ( #14620 ), #8665, .F. ) ;
#4717 = ORIENTED_EDGE ( 'NONE', *, *, #6180, .T. ) ;
#4719 = EDGE_LOOP ( 'NONE', ( #11046, #6665, #6259, #3347 ) ) ;
#4720 = CARTESIAN_POINT ( 'NONE',  ( 82.40000000000000568, -34.78124999877096712, 96.99999999999998579 ) ) ;
#4721 = CARTESIAN_POINT ( 'NONE',  ( -80.90000000000000568, -31.50000000000000000, 97.40192378864668399 ) ) ;
#4722 = ADVANCED_FACE ( 'NONE', ( #11984 ), #4371, .F. ) ;
#4723 = EDGE_CURVE ( 'NONE', #2644, #7081, #2706, .T. ) ;
#4724 = CARTESIAN_POINT ( 'NONE',  ( -82.39999999999999147, -32.30624999877097281, 96.53589838486223584 ) ) ;
#4725 = CARTESIAN_POINT ( 'NONE',  ( 82.39999999999999147, -32.13749999999999574, 96.53589838486223584 ) ) ;
#4726 = CARTESIAN_POINT ( 'NONE',  ( 85.40000000000000568, -33.58124999877097139, 101.7320508075688821 ) ) ;
#4727 = CARTESIAN_POINT ( 'NONE',  ( 229.8435696437499303, -32.84062499938547575, 99.99999999999998579 ) ) ;
#4728 = CARTESIAN_POINT ( 'NONE',  ( 81.02178482187500208, -33.25312499938548427, -102.3871387122750889 ) ) ;
#4729 = DIRECTION ( 'NONE',  ( 0.000000000000000000, 0.000000000000000000, 1.000000000000000000 ) ) ;
#4730 = CARTESIAN_POINT ( 'NONE',  ( 83.77821517812500929, -32.91562499938547859, -97.61286128772489690 ) ) ;
#4731 = VERTEX_POINT ( 'NONE', #4467 ) ;
#4732 = CARTESIAN_POINT ( 'NONE',  ( 235.5999999999999943, -33.41250000000000142, -48.26794919243124582 ) ) ;
#4733 = CARTESIAN_POINT ( 'NONE',  ( -83.20384757729338787, -33.95759618943233704, 102.9999999999999858 ) ) ;
#4734 = CARTESIAN_POINT ( 'NONE',  ( 81.02178482187500208, -32.24062499938548854, -102.3871387122750889 ) ) ;
#4735 =( BOUNDED_CURVE ( )  B_SPLINE_CURVE ( 2, ( #164, #5827, #4261, #13339, #4453, #17648, #16371, #7479, #9036 ),
 .UNSPECIFIED., .F., .F. ) 
 B_SPLINE_CURVE_WITH_KNOTS ( ( 3, 2, 2, 2, 3 ),
 ( 0.3541666666666666297, 0.3611111111111111049, 0.3750000000000000000, 0.3888888888888888951, 0.3958333333333334259 ),
 .UNSPECIFIED. ) 
 CURVE ( )  GEOMETRIC_REPRESENTATION_ITEM ( )  RATIONAL_B_SPLINE_CURVE ( ( 0.9330127018922194093, 0.9330127018922190762, 1.000000000000000000, 0.8660254037844387076, 1.000000000000000000, 0.8660254037844387076, 1.000000000000000000, 0.9330127018922185211, 0.9330127018922192983 ) ) 
 REPRESENTATION_ITEM ( '' )  );
#4736 = CARTESIAN_POINT ( 'NONE',  ( 82.40000000000000568, -30.00000000000000355, 99.99999999999998579 ) ) ;
#4737 = B_SPLINE_CURVE_WITH_KNOTS ( 'NONE', 3,
 ( #10419, #1543, #13823, #7491, #18143, #6033, #3380, #13446, #16383, #12275, #465, #275, #7586, #15197, #4856, #13732 ),
 .UNSPECIFIED., .F., .F.,
 ( 4, 3, 3, 3, 3, 4 ),
 ( -2.111273352581839123E-06, 0.000000000000000000, 3.519286887794243878E-05, 7.191842652046502235E-05, 0.0001049868727088876057, 0.0001382836236814605387 ),
 .UNSPECIFIED. ) ;
#4738 = CARTESIAN_POINT ( 'NONE',  ( -82.39999999999999147, -31.04062499938548569, 103.1828516163667899 ) ) ;
#4739 = CARTESIAN_POINT ( 'NONE',  ( 229.8435696437499871, -32.99062499938548143, -51.59142580818350865 ) ) ;
#4740 = CARTESIAN_POINT ( 'NONE',  ( -81.02178482187500208, -34.79062499938548569, 97.61286128772489690 ) ) ;
#4741 = ORIENTED_EDGE ( 'NONE', *, *, #4115, .F. ) ;
#4742 = CARTESIAN_POINT ( 'NONE',  ( -79.50134204033872720, -34.99892421733355263, 100.8484099402798222 ) ) ;
#4743 = CARTESIAN_POINT ( 'NONE',  ( 235.3564303562499447, -33.92812499938548143, 98.40857419181659793 ) ) ;
#4744 = ADVANCED_FACE ( 'NONE', ( #1634 ), #4562, .F. ) ;
#4745 = CARTESIAN_POINT ( 'NONE',  ( -82.39999999999999147, -32.58750000000000568, 102.9999999999999858 ) ) ;
#4746 = CARTESIAN_POINT ( 'NONE',  ( -85.40000000000000568, -30.90000000000000213, 99.99999999999998579 ) ) ;
#4747 = EDGE_CURVE ( 'NONE', #531, #19282, #13155, .T. ) ;
#4748 = AXIS2_PLACEMENT_3D ( 'NONE', #12398, #9461, #18368 ) ;
#4749 = AXIS2_PLACEMENT_3D ( 'NONE', #10853, #10573, #9007 ) ;
#4750 = CARTESIAN_POINT ( 'NONE',  ( -82.39999999999999147, -34.33124999877097139, 103.0000000000000000 ) ) ;
#4751 = CARTESIAN_POINT ( 'NONE',  ( -79.64356964374998427, -32.31562499938548427, 101.5914258081833879 ) ) ;
#4752 = CARTESIAN_POINT ( 'NONE',  ( 85.14613134194615895, -31.99999999999999289, 100.2978599400813806 ) ) ;
#4753 = CARTESIAN_POINT ( 'NONE',  ( 79.64356964375001269, -34.49062499938548854, 101.5914258081833879 ) ) ;
#4754 = CARTESIAN_POINT ( 'NONE',  ( 81.02178482187500208, -31.75312499938548427, -97.61286128772489690 ) ) ;
#4755 = EDGE_CURVE ( 'NONE', #1228, #18284, #14243, .T. ) ;
#4756 = CARTESIAN_POINT ( 'NONE',  ( 235.3564303562499447, -31.75312499938547717, -48.40857419181671162 ) ) ;
#4757 = CARTESIAN_POINT ( 'NONE',  ( -85.15643035625001289, -32.54062499938548569, 98.40857419181659793 ) ) ;
#4758 = CARTESIAN_POINT ( 'NONE',  ( -81.02178482187500208, -33.25312499938548427, -97.61286128772489690 ) ) ;
#4759 = PRODUCT_DEFINITION_CONTEXT ( 'detailed design', #17572, 'design' ) ;
#4760 = ORIENTED_EDGE ( 'NONE', *, *, #11777, .F. ) ;
#4761 = CARTESIAN_POINT ( 'NONE',  ( 85.40000000000000568, -34.44374999877096855, 99.99999999999998579 ) ) ;
#4762 = CARTESIAN_POINT ( 'NONE',  ( 82.40000000000000568, -30.00000000000000355, -99.99999999999998579 ) ) ;
#4763 = VECTOR ( 'NONE', #6791, 1000.000000000000000 ) ;
#4764 = CYLINDRICAL_SURFACE ( 'NONE', #2093, 3.000000000000002665 ) ;
#4765 = VECTOR ( 'NONE', #14074, 1000.000000000000000 ) ;
#4766 = CARTESIAN_POINT ( 'NONE',  ( -82.39999999999999147, -31.04062499938548569, 103.1828516163667899 ) ) ;
#4767 = CARTESIAN_POINT ( 'NONE',  ( -82.40000000000000568, -30.00000000000000355, -99.99999999999998579 ) ) ;
#4768 = ORIENTED_EDGE ( 'NONE', *, *, #13422, .T. ) ;
#4769 = CARTESIAN_POINT ( 'NONE',  ( -85.40000000000000568, -31.31250000000000000, -98.26794919243111792 ) ) ;
#4770 = CARTESIAN_POINT ( 'NONE',  ( -82.39999999999999147, -32.30624999877096570, 96.99999999999998579 ) ) ;
#4771 = CARTESIAN_POINT ( 'NONE',  ( -82.65333140691201663, -34.99995246259153703, -102.9892844631211943 ) ) ;
#4772 = CARTESIAN_POINT ( 'NONE',  ( -79.64356964375001269, -34.11562499938548854, -98.40857419181659793 ) ) ;
#4773 = CARTESIAN_POINT ( 'NONE',  ( 235.5999999999999375, -32.86874999877096570, -50.00000000000011369 ) ) ;
#4774 = CARTESIAN_POINT ( 'NONE',  ( 229.8435696437499871, -33.81562499938547717, 101.5914258081833879 ) ) ;
#4775 = CARTESIAN_POINT ( 'NONE',  ( -80.90000000000000568, -31.89768749875867471, 97.40192378864668399 ) ) ;
#4776 = EDGE_LOOP ( 'NONE', ( #11438, #13396 ) ) ;
#4777 = CARTESIAN_POINT ( 'NONE',  ( 231.7961524227065979, -32.60759618943232852, 103.0000000000000000 ) ) ;
#4778 = CARTESIAN_POINT ( 'NONE',  ( 85.40000000000000568, -32.21250000000000568, 98.26794919243111792 ) ) ;
#4779 = CARTESIAN_POINT ( 'NONE',  ( 79.64356964374999848, -33.06562499938548427, 99.99999999999998579 ) ) ;
#4780 = AXIS2_PLACEMENT_3D ( 'NONE', #1995, #6593, #2191 ) ;
#4781 = VECTOR ( 'NONE', #8300, 1000.000000000000000 ) ;
#4782 = PLANE ( 'NONE',  #234 ) ;
#4783 = CARTESIAN_POINT ( 'NONE',  ( 85.40000000000000568, -33.05624999877096570, -101.7320508075688679 ) ) ;
#4784 = CARTESIAN_POINT ( 'NONE',  ( 79.39999999999999147, -34.68750000000000000, 101.7320508075688963 ) ) ;
#4785 = ORIENTED_EDGE ( 'NONE', *, *, #11072, .T. ) ;
#4786 = CARTESIAN_POINT ( 'NONE',  ( 235.3564303562499447, -33.21562499938548285, -48.40857419181671162 ) ) ;
#4787 = DIRECTION ( 'NONE',  ( -1.000000000000000000, 0.000000000000000000, 0.000000000000000000 ) ) ;
#4788 = CARTESIAN_POINT ( 'NONE',  ( 235.5999999999999375, -34.66874999877096286, 99.99999999999998579 ) ) ;
#4789 = CARTESIAN_POINT ( 'NONE',  ( 235.3564303562499447, -30.47812499938547859, -50.00000000000011369 ) ) ;
#4790 = LINE ( 'NONE', #6442, #13665 ) ;
#4791 = ORIENTED_EDGE ( 'NONE', *, *, #17646, .F. ) ;
#4792 = VERTEX_POINT ( 'NONE', #10330 ) ;
#4793 = CARTESIAN_POINT ( 'NONE',  ( -82.39999999999999147, -30.25312499938548783, -103.1828516163667899 ) ) ;
#4794 = CIRCLE ( 'NONE', #7888, 9.999999999999998224 ) ;
#4795 =( BOUNDED_CURVE ( )  B_SPLINE_CURVE ( 2, ( #9172, #18172, #3116, #13566, #10268, #1379, #13669 ),
 .UNSPECIFIED., .F., .F. ) 
 B_SPLINE_CURVE_WITH_KNOTS ( ( 3, 2, 2, 3 ),
 ( 0.8958333333333332593, 0.9027777777777777901, 0.9166666666666666297, 0.9258785066912882389 ),
 .UNSPECIFIED. ) 
 CURVE ( )  GEOMETRIC_REPRESENTATION_ITEM ( )  RATIONAL_B_SPLINE_CURVE ( ( 0.9330127018922192983, 0.9330127018922187432, 1.000000000000000000, 0.8660254037844387076, 1.000000000000000000, 0.9111410165655264848, 0.9401539157124900736 ) ) 
 REPRESENTATION_ITEM ( '' )  );
#4796 = CARTESIAN_POINT ( 'NONE',  ( 105.1999999999999744, -29.80000000000000071, -100.0000000000000000 ) ) ;
#4797 = CARTESIAN_POINT ( 'NONE',  ( 4.104070371397484429, -4.047367226856742661, 2.300149018892232304E-16 ) ) ;
#4798 = VERTEX_POINT ( 'NONE', #4179 ) ;
#4799 = LINE ( 'NONE', #10739, #3913 ) ;
#4800 = EDGE_CURVE ( 'NONE', #2988, #15647, #1545, .T. ) ;
#4801 = CARTESIAN_POINT ( 'NONE',  ( -6.259644161404860030E-16, -4.618802153517027165, -3.433295621305388234 ) ) ;
#4802 = CARTESIAN_POINT ( 'NONE',  ( -81.59615242270662350, -33.73259618943233562, 96.99999999999998579 ) ) ;
#4803 = CARTESIAN_POINT ( 'NONE',  ( -79.39999999999999147, -30.65624999877096712, 101.7320508075688537 ) ) ;
#4804 = CARTESIAN_POINT ( 'NONE',  ( -85.40000000000000568, -32.60624999877097707, 101.7320508075688679 ) ) ;
#4805 = DIRECTION ( 'NONE',  ( -0.8660254037844377084, -0.5000000000000015543, 0.000000000000000000 ) ) ;
#4806 = CARTESIAN_POINT ( 'NONE',  ( 5.599999999999999645, 3.061616997868383634E-16, -2.500000000000000444 ) ) ;
#4807 = CARTESIAN_POINT ( 'NONE',  ( -82.40000000000000568, -30.00000000000000355, -103.0000000000000000 ) ) ;
#4808 = CARTESIAN_POINT ( 'NONE',  ( -80.90000000000000568, -34.74374999877097281, -97.40192378864668399 ) ) ;
#4809 = CARTESIAN_POINT ( 'NONE',  ( 233.9782151781249411, -32.54062499938547859, 97.61286128772489690 ) ) ;
#4810 = EDGE_LOOP ( 'NONE', ( #13781, #2165, #18706, #8786 ) ) ;
#4811 = CARTESIAN_POINT ( 'NONE',  ( -79.64356964375001269, -33.47812499938547859, -101.5914258081833879 ) ) ;
#4812 = DIRECTION ( 'NONE',  ( 0.000000000000000000, -1.000000000000000000, 0.000000000000000000 ) ) ;
#4813 = ORIENTED_EDGE ( 'NONE', *, *, #13211, .F. ) ;
#4814 = CARTESIAN_POINT ( 'NONE',  ( -82.40000000000001990, -33.93750000000000711, 103.0000000000000000 ) ) ;
#4815 = FACE_OUTER_BOUND ( 'NONE', #14715, .T. ) ;
#4816 = DIRECTION ( 'NONE',  ( -0.000000000000000000, 0.000000000000000000, -1.000000000000000000 ) ) ;
#4817 = CARTESIAN_POINT ( 'NONE',  ( 96.99999999999994316, -29.80000000000000426, 150.0000000000000000 ) ) ;
#4818 = EDGE_CURVE ( 'NONE', #6898, #14645, #16354, .T. ) ;
#4819 = ORIENTED_EDGE ( 'NONE', *, *, #13543, .F. ) ;
#4820 = ORIENTED_EDGE ( 'NONE', *, *, #19050, .F. ) ;
#4821 = CARTESIAN_POINT ( 'NONE',  ( 81.59615242270662350, -33.41115380933863577, -102.9999999999999858 ) ) ;
#4822 = CARTESIAN_POINT ( 'NONE',  ( 83.77821517812500929, -35.01562499938548711, -102.3871387122750889 ) ) ;
#4823 = CARTESIAN_POINT ( 'NONE',  ( -79.39999999999999147, -32.00624999877096855, 101.7320508075688537 ) ) ;
#4824 = CARTESIAN_POINT ( 'NONE',  ( 82.39999999999999147, -32.81250000000000000, 103.4641016151377499 ) ) ;
#4825 = CARTESIAN_POINT ( 'NONE',  ( -4.154094228333542915, 2.398367420968061658, -3.721909803043254694 ) ) ;
#4826 = CARTESIAN_POINT ( 'NONE',  ( 235.3564303562499447, -34.45312499938548001, 101.5914258081833879 ) ) ;
#4827 = CARTESIAN_POINT ( 'NONE',  ( 79.64356964374998427, -33.59062499938548285, -98.40857419181659793 ) ) ;
#4828 = ADVANCED_FACE ( 'NONE', ( #5938 ), #17856, .F. ) ;
#4829 = CARTESIAN_POINT ( 'NONE',  ( -80.08630547029561342, -32.02340763552836478, -97.87171054440962337 ) ) ;
#4830 = EDGE_CURVE ( 'NONE', #11119, #5593, #6902, .T. ) ;
#4831 = CARTESIAN_POINT ( 'NONE',  ( 82.39999999999999147, -34.07812499938548711, -103.1828516163667899 ) ) ;
#4832 = VERTEX_POINT ( 'NONE', #10708 ) ;
#4833 = CARTESIAN_POINT ( 'NONE',  ( 235.5999999999999943, -31.53749999999999432, -51.73205080756900287 ) ) ;
#4834 = CARTESIAN_POINT ( 'NONE',  ( -79.39999999999999147, -34.31250000000000000, 101.7320508075688537 ) ) ;
#4835 = DIRECTION ( 'NONE',  ( -0.000000000000000000, -0.000000000000000000, -1.000000000000000000 ) ) ;
#4836 = CARTESIAN_POINT ( 'NONE',  ( -83.77821517812500929, -30.77812499938548640, 97.61286128772489690 ) ) ;
#4837 = CARTESIAN_POINT ( 'NONE',  ( 229.8435696437499871, -34.26562499938548001, -48.40857419181671162 ) ) ;
#4838 = CARTESIAN_POINT ( 'NONE',  ( -80.90000000000000568, -30.30000000000000426, 102.5980762113533018 ) ) ;
#4839 = EDGE_CURVE ( 'NONE', #12897, #6852, #9299, .T. ) ;
#4840 = ORIENTED_EDGE ( 'NONE', *, *, #7687, .T. ) ;
#4841 = CARTESIAN_POINT ( 'NONE',  ( 110.9999999999999574, -21.80000000000003268, -139.9999999999999716 ) ) ;
#4842 = CARTESIAN_POINT ( 'NONE',  ( 233.9782151781249411, -34.04062499938547859, 102.3871387122750889 ) ) ;
#4843 = CARTESIAN_POINT ( 'NONE',  ( 85.15643035624999868, -31.00312499938548072, 98.40857419181659793 ) ) ;
#4844 = CARTESIAN_POINT ( 'NONE',  ( -83.77821517812500929, -31.97812499938548925, 102.3871387122750889 ) ) ;
#4845 = CARTESIAN_POINT ( 'NONE',  ( 105.1999999999999744, -34.99999999999999289, -100.0000000000000000 ) ) ;
#4846 = CARTESIAN_POINT ( 'NONE',  ( 81.02178482187500208, -30.89062499938548711, 97.61286128772489690 ) ) ;
#4847 =( REPRESENTATION_RELATIONSHIP ('NONE','NONE', #14468, #19222 ) REPRESENTATION_RELATIONSHIP_WITH_TRANSFORMATION ( #14616 )SHAPE_REPRESENTATION_RELATIONSHIP( ) );
#4848 = CARTESIAN_POINT ( 'NONE',  ( 79.64356964375001269, -31.79062499938548569, -98.40857419181659793 ) ) ;
#4849 = CARTESIAN_POINT ( 'NONE',  ( 235.3564303562499447, -30.81562499938547717, -50.00000000000011369 ) ) ;
#4850 = CARTESIAN_POINT ( 'NONE',  ( -82.39999999999999147, -32.05312499938548854, 96.81714838363319586 ) ) ;
#4851 = CARTESIAN_POINT ( 'NONE',  ( -85.15643035624999868, -33.89062499938548711, -101.5914258081833879 ) ) ;
#4852 = VERTEX_POINT ( 'NONE', #18337 ) ;
#4853 = CARTESIAN_POINT ( 'NONE',  ( 82.39999999999999147, -30.59062499938548640, 96.81714838363319586 ) ) ;
#4854 = CARTESIAN_POINT ( 'NONE',  ( 4.055492966679554279, -2.385006769472701738, -3.005124364834346196 ) ) ;
#4855 = AXIS2_PLACEMENT_3D ( 'NONE', #6523, #2302, #9536 ) ;
#4856 = CARTESIAN_POINT ( 'NONE',  ( 4.082498951862917558, -2.020725942163695166, -3.500000000000000000 ) ) ;
#4857 = CARTESIAN_POINT ( 'NONE',  ( -82.39999999999999147, -35.09062499938548285, 103.1828516163667899 ) ) ;
#4858 = DIRECTION ( 'NONE',  ( -1.000000000000000000, 1.387778780781445676E-15, 2.407412430484046130E-31 ) ) ;
#4859 = ORIENTED_EDGE ( 'NONE', *, *, #2361, .F. ) ;
#4860 = CARTESIAN_POINT ( 'NONE',  ( -82.39999999999999147, -30.11250000000000426, -103.4641016151377499 ) ) ;
#4861 = CARTESIAN_POINT ( 'NONE',  ( 83.90000000000000568, -34.12500000000000000, -97.40192378864668399 ) ) ;
#4862 = CARTESIAN_POINT ( 'NONE',  ( -2.449848172108560540, -3.432307619358754724, -3.503702292528910078 ) ) ;
#4863 = EDGE_CURVE ( 'NONE', #17884, #4491, #4158, .T. ) ;
#4864 = CYLINDRICAL_SURFACE ( 'NONE', #11420, 3.000000000000002665 ) ;
#4865 = CARTESIAN_POINT ( 'NONE',  ( 0.000000000000000000, 0.000000000000000000, 0.000000000000000000 ) ) ;
#4866 = CARTESIAN_POINT ( 'NONE',  ( 232.5999999999999375, -35.09062499938547575, 103.1828516163667899 ) ) ;
#4867 = CARTESIAN_POINT ( 'NONE',  ( -85.40000000000000568, -34.89768749875867826, 99.99999999999998579 ) ) ;
#4868 = ORIENTED_EDGE ( 'NONE', *, *, #14583, .F. ) ;
#4869 = CARTESIAN_POINT ( 'NONE',  ( 82.40000000000000568, -30.00000000000000355, 96.99999999999998579 ) ) ;
#4870 = CARTESIAN_POINT ( 'NONE',  ( 81.59615242270662350, -32.96115380933864003, -103.0000000000000000 ) ) ;
#4871 = CARTESIAN_POINT ( 'NONE',  ( 81.02178482187500208, -34.34062499938548285, 102.3871387122750889 ) ) ;
#4872 = DIRECTION ( 'NONE',  ( -1.000000000000000000, -0.000000000000000000, -0.000000000000000000 ) ) ;
#4873 = VECTOR ( 'NONE', #1423, 1000.000000000000000 ) ;
#4874 = CARTESIAN_POINT ( 'NONE',  ( -83.90000000000000568, -34.51874999877097139, 97.40192378864668399 ) ) ;
#4875 = CARTESIAN_POINT ( 'NONE',  ( 85.40000000000000568, -34.85624999877096997, -101.7320508075688679 ) ) ;
#4876 = CARTESIAN_POINT ( 'NONE',  ( 80.90000000000000568, -34.80000000000000426, 97.40192378864668399 ) ) ;
#4877 = VERTEX_POINT ( 'NONE', #18432 ) ;
#4878 = CARTESIAN_POINT ( 'NONE',  ( 235.3564303562499447, -33.62812499938547717, -50.00000000000011369 ) ) ;
#4879 = CARTESIAN_POINT ( 'NONE',  ( 233.9782151781249411, -31.45312499938548356, 102.3871387122750889 ) ) ;
#4880 = CARTESIAN_POINT ( 'NONE',  ( 232.5999999999999375, -31.49062499938547788, -46.81714838363331666 ) ) ;
#4881 =( GEOMETRIC_REPRESENTATION_CONTEXT ( 3 ) GLOBAL_UNCERTAINTY_ASSIGNED_CONTEXT ( ( #6464 ) ) GLOBAL_UNIT_ASSIGNED_CONTEXT ( ( #8973, #10921, #8378 ) ) REPRESENTATION_CONTEXT ( 'NONE', 'WORKASPACE' ) );
#4882 = EDGE_CURVE ( 'NONE', #15349, #4832, #5050, .T. ) ;
#4883 = CARTESIAN_POINT ( 'NONE',  ( 4.000000000000000000, 2.309401076758515803, -0.4999999999999995559 ) ) ;
#4884 = ORIENTED_EDGE ( 'NONE', *, *, #13096, .F. ) ;
#4885 = ORIENTED_EDGE ( 'NONE', *, *, #13692, .T. ) ;
#4886 = CARTESIAN_POINT ( 'NONE',  ( 3.999999999999999112, 2.309401076758497595, -3.504271511727124366 ) ) ;
#4887 = CARTESIAN_POINT ( 'NONE',  ( -82.39999999999999147, -32.36250000000000426, -102.9999999999999858 ) ) ;
#4888 = CARTESIAN_POINT ( 'NONE',  ( 4.093692494532770176, -4.043567292011561065, 2.300149018892232304E-16 ) ) ;
#4889 = ORIENTED_EDGE ( 'NONE', *, *, #18005, .T. ) ;
#4890 = CARTESIAN_POINT ( 'NONE',  ( -4.000000000000000000, 0.000000000000000000, 0.000000000000000000 ) ) ;
#4891 = CARTESIAN_POINT ( 'NONE',  ( -80.90000000000000568, -34.14374999877097139, -102.5980762113533018 ) ) ;
#4892 = CARTESIAN_POINT ( 'NONE',  ( -80.90000000000000568, -34.20000000000000284, 97.40192378864668399 ) ) ;
#4893 = CARTESIAN_POINT ( 'NONE',  ( -80.90000000000000568, -34.35000000000000853, 102.5980762113533018 ) ) ;
#4894 = CARTESIAN_POINT ( 'NONE',  ( -85.40000000000000568, -33.05624999877096570, 101.7320508075688679 ) ) ;
#4895 = DIRECTION ( 'NONE',  ( 1.387778780781445873E-15, 1.000000000000000000, 0.000000000000000000 ) ) ;
#4896 = CYLINDRICAL_SURFACE ( 'NONE', #17698, 3.000000000000002665 ) ;
#4897 = CARTESIAN_POINT ( 'NONE',  ( 244.7999999999999545, -5.000000000000000888, -103.0000000000000995 ) ) ;
#4898 = CARTESIAN_POINT ( 'NONE',  ( 232.5999999999999375, -33.62812499938547717, 103.1828516163667899 ) ) ;
#4899 = CARTESIAN_POINT ( 'NONE',  ( 235.3564303562499447, -31.26562499938547646, 99.99999999999998579 ) ) ;
#4900 = VERTEX_POINT ( 'NONE', #18145 ) ;
#4901 = CARTESIAN_POINT ( 'NONE',  ( 234.0999999999999375, -31.44374999877096144, 97.40192378864668399 ) ) ;
#4902 = CARTESIAN_POINT ( 'NONE',  ( -79.39999999999999147, -32.83124999877097139, -101.7320508075688963 ) ) ;
#4903 =( BOUNDED_CURVE ( )  B_SPLINE_CURVE ( 2, ( #2425, #7116, #974, #10142, #6929, #16102, #17859, #16296, #7591 ),
 .UNSPECIFIED., .F., .F. ) 
 B_SPLINE_CURVE_WITH_KNOTS ( ( 3, 2, 2, 2, 3 ),
 ( 0.3541666666666666297, 0.3611111111111111049, 0.3750000000000000000, 0.3888888888888888951, 0.3958333333333334259 ),
 .UNSPECIFIED. ) 
 CURVE ( )  GEOMETRIC_REPRESENTATION_ITEM ( )  RATIONAL_B_SPLINE_CURVE ( ( 0.9330127018922194093, 0.9330127018922190762, 1.000000000000000000, 0.8660254037844387076, 1.000000000000000000, 0.8660254037844387076, 1.000000000000000000, 0.9330127018922185211, 0.9330127018922192983 ) ) 
 REPRESENTATION_ITEM ( '' )  );
#4904 = ORIENTED_EDGE ( 'NONE', *, *, #18438, .T. ) ;
#4905 = CARTESIAN_POINT ( 'NONE',  ( -80.90000000000000568, -33.30000000000000426, -102.5980762113533018 ) ) ;
#4906 = CARTESIAN_POINT ( 'NONE',  ( -85.15643035625001289, -30.25312499938548783, 99.99999999999998579 ) ) ;
#4907 = AXIS2_PLACEMENT_3D ( 'NONE', #2469, #11260, #5418 ) ;
#4908 = CYLINDRICAL_SURFACE ( 'NONE', #1632, 3.000000000000009770 ) ;
#4909 = VERTEX_POINT ( 'NONE', #2009 ) ;
#4910 = CARTESIAN_POINT ( 'NONE',  ( 231.7961524227065979, -33.45134618820330275, 103.0000000000000000 ) ) ;
#4911 = B_SPLINE_CURVE_WITH_KNOTS ( 'NONE', 3,
 ( #10005, #2662, #4046, #17725 ),
 .UNSPECIFIED., .F., .F.,
 ( 4, 4 ),
 ( 2.380739282179989060E-07, 0.002044882221487534513 ),
 .UNSPECIFIED. ) ;
#4912 = ORIENTED_EDGE ( 'NONE', *, *, #7854, .F. ) ;
#4913 = ORIENTED_EDGE ( 'NONE', *, *, #3153, .F. ) ;
#4914 = CARTESIAN_POINT ( 'NONE',  ( -84.12306224665888976, -31.99999999999999289, 102.1915028381727382 ) ) ;
#4915 = CARTESIAN_POINT ( 'NONE',  ( 81.02178482187500208, -34.94062499938548427, -102.3871387122750889 ) ) ;
#4916 = DIRECTION ( 'NONE',  ( 0.000000000000000000, -1.000000000000000000, 0.000000000000000000 ) ) ;
#4917 = CARTESIAN_POINT ( 'NONE',  ( -85.40000000000000568, -34.85624999877096997, 101.7320508075688679 ) ) ;
#4918 = CARTESIAN_POINT ( 'NONE',  ( -82.40000000000000568, -50.00000000000000000, 99.99999999999998579 ) ) ;
#4919 = CARTESIAN_POINT ( 'NONE',  ( 82.39999999999999147, -33.43124999877097281, 96.99999999999998579 ) ) ;
#4920 = CARTESIAN_POINT ( 'NONE',  ( 83.77821517812500929, -32.87812499938548427, -102.3871387122750889 ) ) ;
#4921 = ADVANCED_FACE ( 'NONE', ( #3280 ), #13924, .T. ) ;
#4922 = VECTOR ( 'NONE', #9580, 1000.000000000000000 ) ;
#4923 = CARTESIAN_POINT ( 'NONE',  ( 79.39999999999999147, -33.41250000000000142, -101.7320508075688537 ) ) ;
#4924 = CARTESIAN_POINT ( 'NONE',  ( -85.15643035624999868, -33.25312499938548427, 101.5914258081833879 ) ) ;
#4925 = CARTESIAN_POINT ( 'NONE',  ( 85.15643035624999868, -32.80312499938548854, -101.5914258081833879 ) ) ;
#4926 = EDGE_LOOP ( 'NONE', ( #12412, #9584, #5761, #15527 ) ) ;
#4927 = CARTESIAN_POINT ( 'NONE',  ( 229.5999999999999375, -32.73749999999999716, -51.73205080756898866 ) ) ;
#4928 = PRESENTATION_STYLE_ASSIGNMENT (( #18308 ) ) ;
#4929 =( GEOMETRIC_REPRESENTATION_CONTEXT ( 3 ) GLOBAL_UNCERTAINTY_ASSIGNED_CONTEXT ( ( #3528 ) ) GLOBAL_UNIT_ASSIGNED_CONTEXT ( ( #13971, #12894, #5290 ) ) REPRESENTATION_CONTEXT ( 'NONE', 'WORKASPACE' ) );
#4930 = CYLINDRICAL_SURFACE ( 'NONE', #18872, 2.199999999999993516 ) ;
#4931 = CARTESIAN_POINT ( 'NONE',  ( 232.5999999999999943, -32.39062499938548001, 103.1828516163667899 ) ) ;
#4932 = CARTESIAN_POINT ( 'NONE',  ( -83.77821517812500929, -32.42812499938548854, 102.3871387122750889 ) ) ;
#4933 = CARTESIAN_POINT ( 'NONE',  ( 232.5999999999999375, -34.41562499938547859, -53.18285161636690361 ) ) ;
#4934 = CARTESIAN_POINT ( 'NONE',  ( -85.40000000000000568, -32.28750000000000142, 98.26794919243111792 ) ) ;
#4935 = ORIENTED_EDGE ( 'NONE', *, *, #4469, .T. ) ;
#4936 = LINE ( 'NONE', #3359, #5998 ) ;
#4937 = DIRECTION ( 'NONE',  ( 1.000000000000000000, 0.000000000000000000, 0.000000000000000000 ) ) ;
#4938 = FACE_OUTER_BOUND ( 'NONE', #11814, .T. ) ;
#4939 = VECTOR ( 'NONE', #17898, 1000.000000000000000 ) ;
#4940 = VECTOR ( 'NONE', #11546, 1000.000000000000000 ) ;
#4941 = CARTESIAN_POINT ( 'NONE',  ( 229.8306817459156832, -31.99999999999998579, -49.76128878215637741 ) ) ;
#4942 = CARTESIAN_POINT ( 'NONE',  ( -82.39999999999999147, -31.94062499938548427, 103.1828516163667899 ) ) ;
#4943 = CARTESIAN_POINT ( 'NONE',  ( 84.29633955546293578, -32.00000000000002132, 97.97042480180311941 ) ) ;
#4944 = CARTESIAN_POINT ( 'NONE',  ( 82.39999999999999147, -34.64062499938548711, 96.81714838363319586 ) ) ;
#4945 = B_SPLINE_CURVE_WITH_KNOTS ( 'NONE', 3,
 ( #17458, #6821, #3772, #9834, #3872, #7096, #17265, #15987, #8270, #12954 ),
 .UNSPECIFIED., .F., .F.,
 ( 4, 2, 2, 2, 4 ),
 ( 0.3612006186103786654, 0.3925526867148934063, 0.4239047548194081472, 0.4552568229239228881, 0.4866088910284376290 ),
 .UNSPECIFIED. ) ;
#4946 = EDGE_CURVE ( 'NONE', #10357, #4877, #14906, .T. ) ;
#4947 = CARTESIAN_POINT ( 'NONE',  ( 85.15643035624999868, -32.01562499938548711, -101.5914258081833879 ) ) ;
#4948 = VECTOR ( 'NONE', #11090, 1000.000000000000000 ) ;
#4949 = CARTESIAN_POINT ( 'NONE',  ( 235.3564303562499447, -30.32812499938548001, -51.59142580818350865 ) ) ;
#4950 = CARTESIAN_POINT ( 'NONE',  ( -79.64356964374998427, -34.56562499938548427, 101.5914258081833879 ) ) ;
#4951 = CARTESIAN_POINT ( 'NONE',  ( -81.02178482187500208, -34.45312499938548711, -102.3871387122750889 ) ) ;
#4952 = EDGE_LOOP ( 'NONE', ( #13798, #16150, #7809, #347 ) ) ;
#4953 = CARTESIAN_POINT ( 'NONE',  ( 83.77821517812500929, -32.42812499938548854, 97.61286128772489690 ) ) ;
#4954 = CARTESIAN_POINT ( 'NONE',  ( 231.7961524227065695, -32.15759618943231857, 102.9999999999999858 ) ) ;
#4955 = VECTOR ( 'NONE', #15894, 1000.000000000000000 ) ;
#4956 = CARTESIAN_POINT ( 'NONE',  ( -82.39999999999999147, -31.82812499938548356, 103.1828516163667899 ) ) ;
#4957 = CARTESIAN_POINT ( 'NONE',  ( -79.64356964375001269, -34.11562499938548854, 101.5914258081833879 ) ) ;
#4958 = CARTESIAN_POINT ( 'NONE',  ( -82.40000000000000568, -30.00000000000000355, 99.99999999999998579 ) ) ;
#4959 = ORIENTED_EDGE ( 'NONE', *, *, #15335, .F. ) ;
#4960 = CARTESIAN_POINT ( 'NONE',  ( -80.90000000000000568, -32.55000000000000426, -97.40192378864668399 ) ) ;
#4961 = EDGE_CURVE ( 'NONE', #16577, #15956, #10743, .T. ) ;
#4962 = CARTESIAN_POINT ( 'NONE',  ( 105.2000000000000739, -32.00000000000002842, 147.7999999999999829 ) ) ;
#4963 = FACE_OUTER_BOUND ( 'NONE', #715, .T. ) ;
#4964 = CYLINDRICAL_SURFACE ( 'NONE', #7359, 3.000000000000002665 ) ;
#4965 = ADVANCED_FACE ( 'NONE', ( #6229 ), #8071, .F. ) ;
#4966 = CARTESIAN_POINT ( 'NONE',  ( -4.175002511812151873, -2.208363329454905877, -3.469254087858246738 ) ) ;
#4967 = CARTESIAN_POINT ( 'NONE',  ( 231.2217848218749339, -33.47812499938547859, 97.61286128772489690 ) ) ;
#4968 = CARTESIAN_POINT ( 'NONE',  ( -80.90000000000000568, -34.14768749875867826, 97.40192378864668399 ) ) ;
#4969 = APPLICATION_CONTEXT ( 'automotive_design' ) ;
#4970 = EDGE_LOOP ( 'NONE', ( #17911, #2314, #14959, #431 ) ) ;
#4971 = CARTESIAN_POINT ( 'NONE',  ( 99.99999999999997158, -29.80000000000000071, 150.0000000000000000 ) ) ;
#4972 = CARTESIAN_POINT ( 'NONE',  ( -82.39999999999999147, -34.33124999877097139, 103.0000000000000000 ) ) ;
#4973 = FACE_OUTER_BOUND ( 'NONE', #16895, .T. ) ;
#4974 = CARTESIAN_POINT ( 'NONE',  ( 85.40000000000000568, -34.44374999877096855, -99.99999999999998579 ) ) ;
#4975 = PLANE ( 'NONE',  #2756 ) ;
#4976 = CARTESIAN_POINT ( 'NONE',  ( 83.77821517812500929, -32.42812499938548854, -102.3871387122750889 ) ) ;
#4977 = DIRECTION ( 'NONE',  ( -1.000000000000000000, 0.000000000000000000, -0.000000000000000000 ) ) ;
#4978 = ORIENTED_EDGE ( 'NONE', *, *, #3990, .T. ) ;
#4979 = CARTESIAN_POINT ( 'NONE',  ( 80.90000000000000568, -30.69374999877097210, 97.40192378864668399 ) ) ;
#4980 = EDGE_CURVE ( 'NONE', #5083, #11132, #12177, .T. ) ;
#4981 = CARTESIAN_POINT ( 'NONE',  ( 229.8435696437499871, -32.91562499938547859, 101.5914258081833879 ) ) ;
#4982 = CARTESIAN_POINT ( 'NONE',  ( 235.3564303562499447, -31.41562499938548214, -48.40857419181671162 ) ) ;
#4983 = CARTESIAN_POINT ( 'NONE',  ( -85.15643035624999868, -34.22812499938547859, 98.40857419181659793 ) ) ;
#4984 = CARTESIAN_POINT ( 'NONE',  ( -82.39999999999999147, -34.75312499938548427, 96.81714838363319586 ) ) ;
#4985 = VERTEX_POINT ( 'NONE', #373 ) ;
#4986 = ORIENTED_EDGE ( 'NONE', *, *, #13211, .T. ) ;
#4987 = CARTESIAN_POINT ( 'NONE',  ( 4.071447262713887127, -2.020725942163688060, 3.500000000000000444 ) ) ;
#4988 = LINE ( 'NONE', #10931, #19105 ) ;
#4989 = CARTESIAN_POINT ( 'NONE',  ( -83.20384757729338787, -33.95759618943233704, -97.00000000000000000 ) ) ;
#4990 = VERTEX_POINT ( 'NONE', #6325 ) ;
#4991 = CARTESIAN_POINT ( 'NONE',  ( 81.02178482187500208, -32.20312499938548711, 102.3871387122750889 ) ) ;
#4992 = CARTESIAN_POINT ( 'NONE',  ( -83.90000000000000568, -33.01874999877097139, -97.40192378864668399 ) ) ;
#4993 = CARTESIAN_POINT ( 'NONE',  ( 100.0000000000000000, 10.19999999999997620, -139.9999999999999716 ) ) ;
#4994 = CARTESIAN_POINT ( 'NONE',  ( -85.40000000000000568, -32.60624999877097707, 101.7320508075688679 ) ) ;
#4995 = EDGE_CURVE ( 'NONE', #6366, #8755, #12277, .T. ) ;
#4996 = CARTESIAN_POINT ( 'NONE',  ( -79.39999999999999147, -32.90624999877096712, 101.7320508075688537 ) ) ;
#4997 = CARTESIAN_POINT ( 'NONE',  ( 84.75088379147460671, -34.99999999999999289, -101.6079878054130035 ) ) ;
#4998 = CARTESIAN_POINT ( 'NONE',  ( 231.7961524227065695, -33.90134618820329138, -47.00000000000009948 ) ) ;
#4999 = CARTESIAN_POINT ( 'NONE',  ( -79.39999999999999147, -34.18124999877097281, 98.26794919243110371 ) ) ;
#5000 = CARTESIAN_POINT ( 'NONE',  ( 232.5999999999999375, -33.85312499938547859, 96.81714838363319586 ) ) ;
#5001 = EDGE_LOOP ( 'NONE', ( #8223, #18501, #18657, #11880 ) ) ;
#5002 =( LENGTH_UNIT ( ) NAMED_UNIT ( * ) SI_UNIT ( .MILLI., .METRE. ) );
#5003 = ADVANCED_FACE ( 'NONE', ( #10802 ), #16766, .F. ) ;
#5004 = CARTESIAN_POINT ( 'NONE',  ( 232.5999999999999375, -31.18124999877096215, 103.4641016151377499 ) ) ;
#5005 = CARTESIAN_POINT ( 'NONE',  ( 229.5999999999999375, -32.23124999877096286, 98.26794919243111792 ) ) ;
#5006 = ORIENTED_EDGE ( 'NONE', *, *, #8397, .F. ) ;
#5007 = CARTESIAN_POINT ( 'NONE',  ( -82.40000000000000568, -33.65624999877097423, 97.00000000000000000 ) ) ;
#5008 = DIRECTION ( 'NONE',  ( 0.000000000000000000, -1.000000000000000000, 0.000000000000000000 ) ) ;
#5009 = CARTESIAN_POINT ( 'NONE',  ( 229.8377951939018828, -35.00000000000002132, -51.08685357171012242 ) ) ;
#5010 = ORIENTED_EDGE ( 'NONE', *, *, #3978, .F. ) ;
#5011 = CARTESIAN_POINT ( 'NONE',  ( 232.5999999999999375, -34.52812499938548285, -46.81714838363331666 ) ) ;
#5012 = EDGE_LOOP ( 'NONE', ( #14719, #11712 ) ) ;
#5013 = ORIENTED_EDGE ( 'NONE', *, *, #4818, .T. ) ;
#5014 = CARTESIAN_POINT ( 'NONE',  ( -80.42036527867318796, -31.99999999999998579, 102.1983759483903924 ) ) ;
#5015 = CARTESIAN_POINT ( 'NONE',  ( 79.39999999999999147, -30.18750000000000355, -98.26794919243110371 ) ) ;
#5016 = DIRECTION ( 'NONE',  ( 4.415659757031858318E-14, 0.000000000000000000, -1.000000000000000000 ) ) ;
#5017 = CARTESIAN_POINT ( 'NONE',  ( -80.90000000000000568, -34.29374999877096997, 102.5980762113533018 ) ) ;
#5018 = DIRECTION ( 'NONE',  ( 1.000000000000000000, 0.000000000000000000, 0.000000000000000000 ) ) ;
#5019 = CARTESIAN_POINT ( 'NONE',  ( -2.687328764639638656, 3.067272167851286202, -0.05923475698270370959 ) ) ;
#5020 = CARTESIAN_POINT ( 'NONE',  ( 83.77821517812500929, -33.02812499938548285, -97.61286128772489690 ) ) ;
#5021 = DIRECTION ( 'NONE',  ( -1.000000000000000000, 0.000000000000000000, 0.000000000000000000 ) ) ;
#5022 = CARTESIAN_POINT ( 'NONE',  ( -83.77821517812500929, -32.31562499938548427, 102.3871387122750889 ) ) ;
#5023 = CARTESIAN_POINT ( 'NONE',  ( 81.02178482187500208, -34.04062499938548569, -102.3871387122750889 ) ) ;
#5024 = ORIENTED_EDGE ( 'NONE', *, *, #11145, .F. ) ;
#5025 = CARTESIAN_POINT ( 'NONE',  ( 234.0999999999999375, -32.39999999999999858, -52.59807621135342970 ) ) ;
#5026 = CARTESIAN_POINT ( 'NONE',  ( -85.40000000000000568, -34.95000000000000284, 99.99999999999998579 ) ) ;
#5027 = CARTESIAN_POINT ( 'NONE',  ( 82.39999999999999147, -33.48750000000000426, -103.0000000000000000 ) ) ;
#5028 = CARTESIAN_POINT ( 'NONE',  ( 235.3564303562499447, -33.14062499938548001, 98.40857419181659793 ) ) ;
#5029 = CARTESIAN_POINT ( 'NONE',  ( -85.15643035624999868, -32.46562499938548996, 101.5914258081833879 ) ) ;
#5030 = CARTESIAN_POINT ( 'NONE',  ( 231.2217848218749339, -32.57812499938548001, -52.38713871227520968 ) ) ;
#5031 = CARTESIAN_POINT ( 'NONE',  ( -83.90000000000000568, -31.72500000000000142, 102.5980762113533018 ) ) ;
#5032 = ORIENTED_EDGE ( 'NONE', *, *, #6388, .T. ) ;
#5033 = CARTESIAN_POINT ( 'NONE',  ( -85.11055541976942607, -34.99883777075648084, 98.66815749044441475 ) ) ;
#5034 = CARTESIAN_POINT ( 'NONE',  ( 233.4038475772933339, -33.91740381056766296, -47.00000000000011369 ) ) ;
#5035 = CARTESIAN_POINT ( 'NONE',  ( 79.64356964375001269, -33.10312499938549280, 98.40857419181659793 ) ) ;
#5036 = CARTESIAN_POINT ( 'NONE',  ( 84.85729912020865129, -31.99999999999998579, -101.2614033343868414 ) ) ;
#5037 = CARTESIAN_POINT ( 'NONE',  ( -83.77821517812500929, -30.77812499938548640, 97.61286128772489690 ) ) ;
#5038 = CARTESIAN_POINT ( 'NONE',  ( -83.77821517812500929, -32.57812499938548711, -102.3871387122750889 ) ) ;
#5039 = CARTESIAN_POINT ( 'NONE',  ( 82.39999999999999147, -30.25312499938548783, 103.1828516163667899 ) ) ;
#5040 = B_SPLINE_CURVE_WITH_KNOTS ( 'NONE', 3,
 ( #10265, #14743, #1378, #7324, #19252, #5870, #11821, #13760, #113, #10735, #3115, #10929, #9363, #3409, #10830, #16897, #15324, #16512 ),
 .UNSPECIFIED., .F., .F.,
 ( 4, 2, 2, 2, 2, 2, 2, 2, 4 ),
 ( 0.000000000000000000, 0.0007089252359835698227, 0.001417850471967139645, 0.002126775707950709360, 0.002835700943934279291, 0.003544626179917849222, 0.004253551415901418720, 0.004962476651884989085, 0.005671401887868558582 ),
 .UNSPECIFIED. ) ;
#5041 = CARTESIAN_POINT ( 'NONE',  ( 85.15643035624999868, -31.64062499938548356, -98.40857419181659793 ) ) ;
#5042 = CARTESIAN_POINT ( 'NONE',  ( 232.5999999999999091, -33.03749999999998721, -47.00000000000011369 ) ) ;
#5043 = CARTESIAN_POINT ( 'NONE',  ( -79.64356964374998427, -33.14062499938548711, 98.40857419181659793 ) ) ;
#5044 = CARTESIAN_POINT ( 'NONE',  ( -85.15643035624999868, -32.99062499938548854, -101.5914258081833879 ) ) ;
#5045 = VERTEX_POINT ( 'NONE', #11194 ) ;
#5046 = CARTESIAN_POINT ( 'NONE',  ( 81.02178482187500208, -32.35312499938548569, 97.61286128772489690 ) ) ;
#5047 = CARTESIAN_POINT ( 'NONE',  ( 4.180231891692620216, -2.049421325483212097, -3.591231015387277292 ) ) ;
#5048 = CARTESIAN_POINT ( 'NONE',  ( -83.77821517812500929, -30.66562499938548569, 97.61286128772489690 ) ) ;
#5049 = CARTESIAN_POINT ( 'NONE',  ( -82.39999999999999147, -33.51562499938548001, 96.81714838363319586 ) ) ;
#5050 = LINE ( 'NONE', #15200, #3682 ) ;
#5051 = ORIENTED_EDGE ( 'NONE', *, *, #5069, .T. ) ;
#5052 = CARTESIAN_POINT ( 'NONE',  ( -85.40000000000000568, -33.63750000000000284, -101.7320508075688679 ) ) ;
#5053 = EDGE_CURVE ( 'NONE', #13429, #3532, #11173, .T. ) ;
#5054 = EDGE_CURVE ( 'NONE', #2550, #8815, #5143, .T. ) ;
#5055 = CARTESIAN_POINT ( 'NONE',  ( 82.40000000000000568, -30.00000000000000355, -99.99999999999998579 ) ) ;
#5056 = CARTESIAN_POINT ( 'NONE',  ( 84.57144699476174310, -35.00000000000000000, -97.92073041325133431 ) ) ;
#5057 = LINE ( 'NONE', #5149, #2987 ) ;
#5058 = CARTESIAN_POINT ( 'NONE',  ( 231.2217848218749339, -34.67812499938548143, 102.3871387122750889 ) ) ;
#5059 = CARTESIAN_POINT ( 'NONE',  ( -79.39999999999999147, -33.73518749875868394, 98.26794919243110371 ) ) ;
#5060 = ORIENTED_EDGE ( 'NONE', *, *, #7076, .F. ) ;
#5061 = LINE ( 'NONE', #11099, #17114 ) ;
#5062 = CARTESIAN_POINT ( 'NONE',  ( -85.40000000000000568, -34.40624999877096712, 101.7320508075688821 ) ) ;
#5063 = DIRECTION ( 'NONE',  ( -1.000000000000000000, 0.000000000000000000, 0.000000000000000000 ) ) ;
#5064 = CARTESIAN_POINT ( 'NONE',  ( 82.39999999999999147, -34.33124999877097139, -103.0000000000000000 ) ) ;
#5065 = CARTESIAN_POINT ( 'NONE',  ( 82.39999999999999147, -30.36562499938549209, -96.81714838363319586 ) ) ;
#5066 = EDGE_CURVE ( 'NONE', #4350, #6967, #14212, .T. ) ;
#5067 = CARTESIAN_POINT ( 'NONE',  ( 231.0999999999999375, -34.87499999999999289, 102.5980762113533018 ) ) ;
#5068 = AXIS2_PLACEMENT_3D ( 'NONE', #13206, #1492, #13020 ) ;
#5069 = EDGE_CURVE ( 'NONE', #16231, #16006, #17452, .T. ) ;
#5070 = ORIENTED_EDGE ( 'NONE', *, *, #9476, .F. ) ;
#5071 = CARTESIAN_POINT ( 'NONE',  ( 82.39999999999999147, -30.73124999877096641, 96.53589838486223584 ) ) ;
#5072 = SHAPE_DEFINITION_REPRESENTATION ( #3898, #7631 ) ;
#5073 = CARTESIAN_POINT ( 'NONE',  ( 235.3564303562499447, -33.62812499938547717, 99.99999999999998579 ) ) ;
#5074 = EDGE_CURVE ( 'NONE', #17889, #15031, #8977, .T. ) ;
#5075 = CARTESIAN_POINT ( 'NONE',  ( 232.5999999999999375, -30.59062499938547930, -46.81714838363331666 ) ) ;
#5076 = CARTESIAN_POINT ( 'NONE',  ( -81.02178482187500208, -32.54062499938548569, 97.61286128772489690 ) ) ;
#5077 = LINE ( 'NONE', #17082, #15230 ) ;
#5078 = VERTEX_POINT ( 'NONE', #5348 ) ;
#5079 = ORIENTED_EDGE ( 'NONE', *, *, #6126, .F. ) ;
#5080 = CARTESIAN_POINT ( 'NONE',  ( -82.39999999999999147, -32.27812499938548285, -96.81714838363319586 ) ) ;
#5081 = CARTESIAN_POINT ( 'NONE',  ( -85.40000000000000568, -32.28750000000000142, -101.7320508075688821 ) ) ;
#5082 = CARTESIAN_POINT ( 'NONE',  ( 105.2000000000000455, -29.80000000000002203, 147.7999999999999829 ) ) ;
#5083 = VERTEX_POINT ( 'NONE', #9927 ) ;
#5084 = CARTESIAN_POINT ( 'NONE',  ( -85.40000000000000568, -34.03124999877096712, -101.7320508075688679 ) ) ;
#5085 = VECTOR ( 'NONE', #3634, 1000.000000000000000 ) ;
#5086 = CARTESIAN_POINT ( 'NONE',  ( -79.39999999999999147, -34.23750000000000426, 98.26794919243110371 ) ) ;
#5087 = CARTESIAN_POINT ( 'NONE',  ( -83.90000000000000568, -32.56874999877096855, 102.5980762113533018 ) ) ;
#5088 = CARTESIAN_POINT ( 'NONE',  ( -79.39999999999999147, -35.15624999877096712, 101.7320508075688537 ) ) ;
#5089 = CARTESIAN_POINT ( 'NONE',  ( 96.99999999999997158, -5.200000000000003730, -150.0000000000000000 ) ) ;
#5090 = FACE_BOUND ( 'NONE', #1083, .T. ) ;
#5091 = CARTESIAN_POINT ( 'NONE',  ( 85.40000000000000568, -30.43124999877096926, -98.26794919243111792 ) ) ;
#5092 = CARTESIAN_POINT ( 'NONE',  ( 235.3564303562499447, -33.96562499938547575, 99.99999999999998579 ) ) ;
#5093 = ORIENTED_EDGE ( 'NONE', *, *, #782, .F. ) ;
#5094 = CARTESIAN_POINT ( 'NONE',  ( 82.39999999999999147, -32.05312499938548854, -96.81714838363319586 ) ) ;
#5095 = SURFACE_SIDE_STYLE ('',( #2052 ) ) ;
#5096 = CARTESIAN_POINT ( 'NONE',  ( 234.0999999999999375, -30.69374999877096499, 102.5980762113533018 ) ) ;
#5097 = CARTESIAN_POINT ( 'NONE',  ( 4.104070371397481765, 4.047367226856737332, -1.119160662980175398E-16 ) ) ;
#5098 = AXIS2_PLACEMENT_3D ( 'NONE', #2939, #19264, #15144 ) ;
#5099 = EDGE_LOOP ( 'NONE', ( #4538, #17421, #7613, #1660 ) ) ;
#5100 = CARTESIAN_POINT ( 'NONE',  ( -85.40000000000000568, -33.54374999877096286, 99.99999999999998579 ) ) ;
#5101 = DIRECTION ( 'NONE',  ( -0.000000000000000000, -0.000000000000000000, 1.000000000000000000 ) ) ;
#5102 = UNCERTAINTY_MEASURE_WITH_UNIT (LENGTH_MEASURE( 1.000000000000000082E-05 ), #14163, 'distance_accuracy_value', 'NONE');
#5103 = CARTESIAN_POINT ( 'NONE',  ( 99.99999999999994316, -29.80000000000000782, -150.0000000000000000 ) ) ;
#5104 = ORIENTED_EDGE ( 'NONE', *, *, #11016, .F. ) ;
#5105 = DIRECTION ( 'NONE',  ( -0.000000000000000000, 0.000000000000000000, -1.000000000000000000 ) ) ;
#5106 = CARTESIAN_POINT ( 'NONE',  ( 4.165266963751927065, -2.049631966911921843, 3.550066703508780286 ) ) ;
#5107 = VERTEX_POINT ( 'NONE', #1131 ) ;
#5108 = CARTESIAN_POINT ( 'NONE',  ( -79.79666399293490997, -31.99999999999999289, 101.4892189721554416 ) ) ;
#5109 = CARTESIAN_POINT ( 'NONE',  ( 82.39999999999999147, -34.75312499938549138, -96.81714838363319586 ) ) ;
#5110 = CARTESIAN_POINT ( 'NONE',  ( -4.000000000000000000, -0.7890432684750890990, -0.04868663549882315533 ) ) ;
#5111 = CARTESIAN_POINT ( 'NONE',  ( -83.77821517812500929, -30.32812499938548711, 97.61286128772489690 ) ) ;
#5112 = CARTESIAN_POINT ( 'NONE',  ( -79.39999999999999147, -34.23356250001229739, 98.26794919243110371 ) ) ;
#5113 = EDGE_CURVE ( 'NONE', #15126, #12906, #12145, .T. ) ;
#5114 = UNCERTAINTY_MEASURE_WITH_UNIT (LENGTH_MEASURE( 1.000000000000000082E-05 ), #17999, 'distance_accuracy_value', 'NONE');
#5115 = CARTESIAN_POINT ( 'NONE',  ( 79.39999999999999147, -33.28124999877096712, 101.7320508075688963 ) ) ;
#5116 = CARTESIAN_POINT ( 'NONE',  ( 85.15643035625001289, -32.05312499938548854, -99.99999999999998579 ) ) ;
#5117 = LINE ( 'NONE', #11057, #4323 ) ;
#5118 = CARTESIAN_POINT ( 'NONE',  ( -83.77821517812500929, -34.11562499938548854, 102.3871387122750889 ) ) ;
#5119 = CARTESIAN_POINT ( 'NONE',  ( 85.15643035624999868, -34.60312499938548569, -101.5914258081833879 ) ) ;
#5120 = ORIENTED_EDGE ( 'NONE', *, *, #17523, .T. ) ;
#5121 = CARTESIAN_POINT ( 'NONE',  ( 232.5999999999999375, -34.61249999999999716, 97.00000000000000000 ) ) ;
#5122 = SURFACE_SIDE_STYLE ('',( #11063 ) ) ;
#5123 = CARTESIAN_POINT ( 'NONE',  ( 113.6225952641917161, 11.47451905283827855, 50.00000000000001421 ) ) ;
#5124 = CARTESIAN_POINT ( 'NONE',  ( -81.02178482187500208, -31.00312499938548783, 102.3871387122750889 ) ) ;
#5125 = CARTESIAN_POINT ( 'NONE',  ( 233.9782151781249411, -33.10312499938547859, -52.38713871227520968 ) ) ;
#5126 = CARTESIAN_POINT ( 'NONE',  ( -85.40000000000000568, -32.25000000000000000, 99.99999999999998579 ) ) ;
#5127 = ORIENTED_EDGE ( 'NONE', *, *, #17486, .F. ) ;
#5128 = CARTESIAN_POINT ( 'NONE',  ( 3.950250160040163383, -0.7258013381034684741, 3.499999999999845013 ) ) ;
#5129 = CARTESIAN_POINT ( 'NONE',  ( 235.5999999999999375, -33.82499999999999574, -50.00000000000011369 ) ) ;
#5130 = CARTESIAN_POINT ( 'NONE',  ( 81.02178482187500208, -33.44062499938548427, 102.3871387122750889 ) ) ;
#5131 = CARTESIAN_POINT ( 'NONE',  ( 79.39999999999999147, -32.06250000000000000, -101.7320508075688537 ) ) ;
#5132 = CARTESIAN_POINT ( 'NONE',  ( -85.15643035625001289, -31.19062499938548783, 98.40857419181659793 ) ) ;
#5133 = CARTESIAN_POINT ( 'NONE',  ( 80.80636817121803972, -32.00000000000000000, 97.53037344451318802 ) ) ;
#5134 = CARTESIAN_POINT ( 'NONE',  ( 83.77821517812500929, -31.11562499938548498, 102.3871387122750889 ) ) ;
#5135 = CARTESIAN_POINT ( 'NONE',  ( 85.15643035624999868, -30.74062499938548143, -98.40857419181659793 ) ) ;
#5136 = CARTESIAN_POINT ( 'NONE',  ( 232.5999999999999375, -30.47812499938547859, -46.81714838363331666 ) ) ;
#5137 = CARTESIAN_POINT ( 'NONE',  ( -79.64356964374999848, -33.62812499938548427, 99.99999999999998579 ) ) ;
#5138 = CARTESIAN_POINT ( 'NONE',  ( -81.02178482187500208, -34.00312499938548427, -102.3871387122750889 ) ) ;
#5139 = ORIENTED_EDGE ( 'NONE', *, *, #16654, .T. ) ;
#5140 = CARTESIAN_POINT ( 'NONE',  ( 81.02178482187500208, -31.90312499938548996, 97.61286128772489690 ) ) ;
#5141 = CARTESIAN_POINT ( 'NONE',  ( 3.948103430090712962, -3.379418997638331312, -1.146674596027277060 ) ) ;
#5142 = CARTESIAN_POINT ( 'NONE',  ( -85.15643035624999868, -33.36562499938548854, 101.5914258081833879 ) ) ;
#5143 = LINE ( 'NONE', #11385, #16797 ) ;
#5144 = B_SPLINE_CURVE_WITH_KNOTS ( 'NONE', 3,
 ( #1327, #16269, #19104, #5919, #1522, #6009 ),
 .UNSPECIFIED., .F., .F.,
 ( 4, 2, 4 ),
 ( -3.640115492409406142E-06, 0.0002066546034003385283, 0.0004169493222930864334 ),
 .UNSPECIFIED. ) ;
#5145 = ORIENTED_EDGE ( 'NONE', *, *, #13454, .T. ) ;
#5146 = CARTESIAN_POINT ( 'NONE',  ( -83.90000000000000568, -34.42500000000000426, -97.40192378864668399 ) ) ;
#5147 = CARTESIAN_POINT ( 'NONE',  ( -81.59615242270663771, -32.51115380933863008, 103.0000000000000000 ) ) ;
#5148 = DIRECTION ( 'NONE',  ( -0.000000000000000000, -1.000000000000000000, -0.000000000000000000 ) ) ;
#5149 = CARTESIAN_POINT ( 'NONE',  ( 99.99999999999994316, -32.00000000000000000, 150.0000000000000000 ) ) ;
#5150 = CARTESIAN_POINT ( 'NONE',  ( 231.2217848218749339, -34.37812499938547717, 97.61286128772489690 ) ) ;
#5151 = CARTESIAN_POINT ( 'NONE',  ( -79.39999999999999147, -35.12268749875867258, 99.99999999999998579 ) ) ;
#5152 = ORIENTED_EDGE ( 'NONE', *, *, #8633, .F. ) ;
#5153 = CARTESIAN_POINT ( 'NONE',  ( -83.77821517812500929, -35.12812499938548427, 102.3871387122750889 ) ) ;
#5154 = PLANE ( 'NONE',  #10387 ) ;
#5155 = CARTESIAN_POINT ( 'NONE',  ( -85.40000000000000568, -33.18750000000000000, 98.26794919243111792 ) ) ;
#5156 = CARTESIAN_POINT ( 'NONE',  ( 83.77821517812500929, -30.77812499938548640, 102.3871387122750889 ) ) ;
#5157 = CARTESIAN_POINT ( 'NONE',  ( -82.40000000000000568, -30.00000000000000355, 99.99999999999998579 ) ) ;
#5158 = CARTESIAN_POINT ( 'NONE',  ( 85.15643035624999868, -31.56562499938548427, -101.5914258081833879 ) ) ;
#5159 = DIRECTION ( 'NONE',  ( 0.000000000000000000, 0.000000000000000000, -1.000000000000000000 ) ) ;
#5160 = VECTOR ( 'NONE', #15747, 1000.000000000000000 ) ;
#5161 = ORIENTED_EDGE ( 'NONE', *, *, #54, .T. ) ;
#5162 = CARTESIAN_POINT ( 'NONE',  ( 85.40000000000000568, -31.78124999877096712, 101.7320508075688679 ) ) ;
#5163 = APPLICATION_PROTOCOL_DEFINITION ( 'draft international standard', 'automotive_design', 1998, #1844 ) ;
#5164 = CARTESIAN_POINT ( 'NONE',  ( 229.8435696437499303, -33.40312499938547575, 99.99999999999998579 ) ) ;
#5165 = CARTESIAN_POINT ( 'NONE',  ( 233.9782151781249411, -33.25312499938547717, -47.61286128772501769 ) ) ;
#5166 = CARTESIAN_POINT ( 'NONE',  ( -81.02178482187500208, -33.14062499938548711, 102.3871387122750889 ) ) ;
#5167 = CARTESIAN_POINT ( 'NONE',  ( 105.2000000000001307, -29.80000000000002203, 153.0000000000000000 ) ) ;
#5168 = VERTEX_POINT ( 'NONE', #14498 ) ;
#5169 = ORIENTED_EDGE ( 'NONE', *, *, #9337, .T. ) ;
#5170 = CARTESIAN_POINT ( 'NONE',  ( -82.39999999999999147, -30.92812499938548143, -96.81714838363319586 ) ) ;
#5171 = DIRECTION ( 'NONE',  ( 1.000000000000000000, 0.000000000000000000, 0.000000000000000000 ) ) ;
#5172 = VERTEX_POINT ( 'NONE', #6812 ) ;
#5173 = CARTESIAN_POINT ( 'NONE',  ( 85.15643035625001289, -32.95312499938548711, 99.99999999999998579 ) ) ;
#5174 = CARTESIAN_POINT ( 'NONE',  ( -80.90000000000000568, -33.84374999877096712, -97.40192378864668399 ) ) ;
#5175 = VECTOR ( 'NONE', #12765, 1000.000000000000000 ) ;
#5176 = FACE_OUTER_BOUND ( 'NONE', #139, .T. ) ;
#5177 = LINE ( 'NONE', #11123, #2881 ) ;
#5178 = CARTESIAN_POINT ( 'NONE',  ( -83.90000000000000568, -31.66874999877096997, 102.5980762113533018 ) ) ;
#5179 =( BOUNDED_CURVE ( )  B_SPLINE_CURVE ( 2, ( #7944, #636, #16740, #9310, #6490, #13896, #15273, #7847, #10874 ),
 .UNSPECIFIED., .F., .F. ) 
 B_SPLINE_CURVE_WITH_KNOTS ( ( 3, 2, 2, 2, 3 ),
 ( 0.1458333333333333426, 0.1527777777777777901, 0.1666666666666666574, 0.1805555555555555525, 0.1875000000000000000 ),
 .UNSPECIFIED. ) 
 CURVE ( )  GEOMETRIC_REPRESENTATION_ITEM ( )  RATIONAL_B_SPLINE_CURVE ( ( 0.9330127018922194093, 0.9330127018922194093, 1.000000000000000000, 0.8660254037844387076, 1.000000000000000000, 0.8660254037844387076, 1.000000000000000000, 0.9330127018922194093, 0.9330127018922194093 ) ) 
 REPRESENTATION_ITEM ( '' )  );
#5180 = CARTESIAN_POINT ( 'NONE',  ( -85.40000000000000568, -33.99374999877097281, 99.99999999999998579 ) ) ;
#5181 = DIRECTION ( 'NONE',  ( 0.000000000000000000, 0.000000000000000000, -1.000000000000000000 ) ) ;
#5182 = DIRECTION ( 'NONE',  ( 1.387778780781445676E-15, 1.000000000000000000, 0.000000000000000000 ) ) ;
#5183 = CARTESIAN_POINT ( 'NONE',  ( 82.39999999999999147, -30.50624999877097210, -96.53589838486223584 ) ) ;
#5184 = CARTESIAN_POINT ( 'NONE',  ( 231.2217848218749339, -33.21562499938547575, 102.3871387122750889 ) ) ;
#5185 = EDGE_CURVE ( 'NONE', #13728, #18169, #14403, .T. ) ;
#5186 = EDGE_LOOP ( 'NONE', ( #12551, #1376, #18250, #5684 ) ) ;
#5187 = CARTESIAN_POINT ( 'NONE',  ( 83.77821517812500929, -33.66562499938548569, -102.3871387122750889 ) ) ;
#5188 = CARTESIAN_POINT ( 'NONE',  ( 105.5000000000000142, 12.69999999999998508, 110.0000000000000142 ) ) ;
#5189 = CARTESIAN_POINT ( 'NONE',  ( -82.39999999999999147, -32.98124999877096286, -96.99999999999998579 ) ) ;
#5190 = ORIENTED_EDGE ( 'NONE', *, *, #12122, .F. ) ;
#5191 = AXIS2_PLACEMENT_3D ( 'NONE', #3440, #18490, #2171 ) ;
#5192 = LINE ( 'NONE', #16914, #4922 ) ;
#5193 = CARTESIAN_POINT ( 'NONE',  ( 79.58826230851033756, -31.99999999999998579, -98.95399275611669054 ) ) ;
#5194 = CARTESIAN_POINT ( 'NONE',  ( -0.6937372685066653943, 4.453844082567723461, -3.610536846335889116 ) ) ;
#5195 = VERTEX_POINT ( 'NONE', #4063 ) ;
#5196 = CARTESIAN_POINT ( 'NONE',  ( -82.39999999999999147, -31.85624999877096641, 96.99999999999998579 ) ) ;
#5197 = CARTESIAN_POINT ( 'NONE',  ( -81.59615242270662350, -33.67634618820330417, 96.99999999999997158 ) ) ;
#5198 = VERTEX_POINT ( 'NONE', #1042 ) ;
#5199 = LINE ( 'NONE', #6767, #6350 ) ;
#5200 = ADVANCED_FACE ( 'NONE', ( #5539 ), #18825, .F. ) ;
#5201 = CARTESIAN_POINT ( 'NONE',  ( 85.40000000000000568, -30.86250000000000071, -101.7320508075688679 ) ) ;
#5202 = FACE_OUTER_BOUND ( 'NONE', #5186, .T. ) ;
#5203 = AXIS2_PLACEMENT_3D ( 'NONE', #3403, #16792, #9356 ) ;
#5204 = EDGE_CURVE ( 'NONE', #4595, #10520, #12770, .T. ) ;
#5205 = CARTESIAN_POINT ( 'NONE',  ( -85.40000000000000568, -33.50624999877096855, 101.7320508075688679 ) ) ;
#5206 = CARTESIAN_POINT ( 'NONE',  ( -85.40000000000000568, -34.49606250001229313, 99.99999999999998579 ) ) ;
#5207 = CARTESIAN_POINT ( 'NONE',  ( -83.90000000000000568, -32.26874999877097139, -102.5980762113533018 ) ) ;
#5208 = CARTESIAN_POINT ( 'NONE',  ( 229.8435696437499303, -35.09062499938547575, 99.99999999999998579 ) ) ;
#5209 = ADVANCED_FACE ( 'NONE', ( #17158 ), #849, .T. ) ;
#5210 = CARTESIAN_POINT ( 'NONE',  ( 79.64356964374998427, -34.56562499938548427, -101.5914258081833879 ) ) ;
#5211 = CARTESIAN_POINT ( 'NONE',  ( -80.90000000000000568, -33.69374999877096855, 97.40192378864668399 ) ) ;
#5212 = CARTESIAN_POINT ( 'NONE',  ( -85.15643035625001289, -33.29062499938547859, 99.99999999999998579 ) ) ;
#5213 = LINE ( 'NONE', #17320, #871 ) ;
#5214 = ORIENTED_EDGE ( 'NONE', *, *, #13730, .T. ) ;
#5215 = CARTESIAN_POINT ( 'NONE',  ( 232.5999999999999375, -33.93750000000000000, -46.53589838486234953 ) ) ;
#5216 = CARTESIAN_POINT ( 'NONE',  ( -84.69814068649969840, -35.00052333152936512, 98.07164593887567605 ) ) ;
#5217 = CARTESIAN_POINT ( 'NONE',  ( 232.5999999999999375, -29.99999999999999645, 99.99999999999998579 ) ) ;
#5218 = CARTESIAN_POINT ( 'NONE',  ( 233.9782151781249411, -32.35312499938547859, 102.3871387122750889 ) ) ;
#5219 = CARTESIAN_POINT ( 'NONE',  ( -79.64356964375001269, -33.21562499938548996, 101.5914258081833879 ) ) ;
#5220 = ADVANCED_FACE ( 'NONE', ( #2298 ), #8672, .F. ) ;
#5221 = CARTESIAN_POINT ( 'NONE',  ( 235.3564303562499447, -30.36562499938547788, -50.00000000000011369 ) ) ;
#5222 = VECTOR ( 'NONE', #3126, 1000.000000000000000 ) ;
#5223 = EDGE_LOOP ( 'NONE', ( #11320, #18728, #3955, #9066, #3118, #4395 ) ) ;
#5224 =( REPRESENTATION_RELATIONSHIP ('NONE','NONE', #14468, #16991 ) REPRESENTATION_RELATIONSHIP_WITH_TRANSFORMATION ( #1247 )SHAPE_REPRESENTATION_RELATIONSHIP( ) );
#5225 = CARTESIAN_POINT ( 'NONE',  ( 0.1388410611046075049, 2.351840044243034722, -2.926493552096022466 ) ) ;
#5226 = FACE_OUTER_BOUND ( 'NONE', #12395, .T. ) ;
#5227 = CARTESIAN_POINT ( 'NONE',  ( 85.15643035624999868, -31.90312499938548285, 98.40857419181659793 ) ) ;
#5228 = CIRCLE ( 'NONE', #7089, 4.000000000000000000 ) ;
#5229 = CARTESIAN_POINT ( 'NONE',  ( 82.40000000000001990, -32.13750000000000284, -103.0000000000000000 ) ) ;
#5230 = ADVANCED_FACE ( 'NONE', ( #11288 ), #4008, .T. ) ;
#5231 = CARTESIAN_POINT ( 'NONE',  ( -85.15643035625001289, -33.89062499938548711, 98.40857419181659793 ) ) ;
#5232 = AXIS2_PLACEMENT_3D ( 'NONE', #6966, #9796, #18700 ) ;
#5233 = DIRECTION ( 'NONE',  ( -0.000000000000000000, -0.000000000000000000, 1.000000000000000000 ) ) ;
#5234 = CARTESIAN_POINT ( 'NONE',  ( 79.64356964374999848, -31.71562499938548285, 99.99999999999998579 ) ) ;
#5235 = CARTESIAN_POINT ( 'NONE',  ( 85.15643035624999868, -34.26562499938548711, -101.5914258081833879 ) ) ;
#5236 = CARTESIAN_POINT ( 'NONE',  ( 232.5999999999999375, -33.40312499938547575, -53.18285161636690361 ) ) ;
#5237 = CARTESIAN_POINT ( 'NONE',  ( -79.64356964374999848, -34.52812499938548285, 99.99999999999998579 ) ) ;
#5238 = CARTESIAN_POINT ( 'NONE',  ( -82.39999999999999147, -31.15312499938548640, -103.1828516163667899 ) ) ;
#5239 = ORIENTED_EDGE ( 'NONE', *, *, #12059, .F. ) ;
#5240 = CARTESIAN_POINT ( 'NONE',  ( 81.02178482187500208, -32.20312499938548711, 102.3871387122750889 ) ) ;
#5241 = CARTESIAN_POINT ( 'NONE',  ( 3.436319922986518449, -2.634841920959471562, -3.531542292954761741 ) ) ;
#5242 = CARTESIAN_POINT ( 'NONE',  ( -79.39999999999999147, -32.47500000000000142, 99.99999999999998579 ) ) ;
#5243 = CARTESIAN_POINT ( 'NONE',  ( -82.39999999999999147, -30.70312499938548711, 96.81714838363319586 ) ) ;
#5244 = CARTESIAN_POINT ( 'NONE',  ( -85.15643035624999868, -32.91562499938549280, 101.5914258081833879 ) ) ;
#5245 = ORIENTED_EDGE ( 'NONE', *, *, #13574, .F. ) ;
#5246 = CARTESIAN_POINT ( 'NONE',  ( -85.40000000000000568, -33.60000000000000142, -99.99999999999998579 ) ) ;
#5247 = VECTOR ( 'NONE', #1252, 1000.000000000000000 ) ;
#5248 =( BOUNDED_CURVE ( )  B_SPLINE_CURVE ( 2, ( #9278, #11757, #13679, #13121, #12123, #19092, #16524, #18093, #13772 ),
 .UNSPECIFIED., .F., .T. ) 
 B_SPLINE_CURVE_WITH_KNOTS ( ( 3, 2, 2, 2, 3 ),
 ( 0.6875000000000000000, 0.6944444444444444198, 0.7083333333333333703, 0.7222222222222222099, 0.7291666666666668517 ),
 .UNSPECIFIED. ) 
 CURVE ( )  GEOMETRIC_REPRESENTATION_ITEM ( )  RATIONAL_B_SPLINE_CURVE ( ( 0.9330127018922194093, 0.9330127018922194093, 1.000000000000000000, 0.8660254037844387076, 1.000000000000000000, 0.8660254037844387076, 1.000000000000000000, 0.9330127018922177440, 0.9330127018922194093 ) ) 
 REPRESENTATION_ITEM ( '' )  );
#5249 = B_SPLINE_CURVE_WITH_KNOTS ( 'NONE', 3,
 ( #11094, #17063, #3678, #15603, #2210, #14120, #759, #12658, #11198, #11772 ),
 .UNSPECIFIED., .F., .F.,
 ( 4, 2, 2, 2, 4 ),
 ( 0.3612006186103786654, 0.3925526867148934063, 0.4239047548194081472, 0.4552568229239228881, 0.4866088910284376290 ),
 .UNSPECIFIED. ) ;
#5250 = VECTOR ( 'NONE', #17752, 1000.000000000000000 ) ;
#5251 = CARTESIAN_POINT ( 'NONE',  ( 80.90000000000000568, -33.00000000000000000, -102.5980762113533018 ) ) ;
#5252 = DIRECTION ( 'NONE',  ( 1.000000000000000000, -1.577021341797101948E-15, 0.000000000000000000 ) ) ;
#5253 = CARTESIAN_POINT ( 'NONE',  ( -82.39999999999999147, -30.55856250001229668, 96.53589838486223584 ) ) ;
#5254 = CARTESIAN_POINT ( 'NONE',  ( 231.2217848218749339, -32.46562499938547575, 97.61286128772489690 ) ) ;
#5255 = CARTESIAN_POINT ( 'NONE',  ( -80.90000000000000568, -34.29768749875867684, 102.5980762113533018 ) ) ;
#5256 = AXIS2_PLACEMENT_3D ( 'NONE', #6926, #11413, #2512 ) ;
#5257 = B_SPLINE_CURVE_WITH_KNOTS ( 'NONE', 1,
 ( #805, #14171 ),
 .UNSPECIFIED., .F., .F.,
 ( 2, 2 ),
 ( 0.000000000000000000, 1.000000000000000000 ),
 .UNSPECIFIED. ) ;
#5258 = CARTESIAN_POINT ( 'NONE',  ( -83.32052461991715120, -34.98323688327303671, 97.06736352196708140 ) ) ;
#5259 = CARTESIAN_POINT ( 'NONE',  ( -85.15643035625001289, -30.14062499938548711, 99.99999999999998579 ) ) ;
#5260 = CARTESIAN_POINT ( 'NONE',  ( 249.9999999999999716, -29.80000000000000426, -100.0000000000000000 ) ) ;
#5261 = CARTESIAN_POINT ( 'NONE',  ( 85.15643035624999868, -30.29062499938548925, 101.5914258081833879 ) ) ;
#5262 = CARTESIAN_POINT ( 'NONE',  ( -85.40000000000000568, -34.44374999877096855, 99.99999999999998579 ) ) ;
#5263 = LINE ( 'NONE', #12772, #16194 ) ;
#5264 = CARTESIAN_POINT ( 'NONE',  ( 85.15643035624999868, -32.09062499938548996, -98.40857419181659793 ) ) ;
#5265 = VECTOR ( 'NONE', #18444, 1000.000000000000000 ) ;
#5266 = CARTESIAN_POINT ( 'NONE',  ( 82.40000000000001990, -32.75624999877096855, 103.0000000000000000 ) ) ;
#5267 = ORIENTED_EDGE ( 'NONE', *, *, #7090, .T. ) ;
#5268 = CARTESIAN_POINT ( 'NONE',  ( 85.40000000000000568, -31.74374999877096926, 99.99999999999998579 ) ) ;
#5269 = APPLICATION_PROTOCOL_DEFINITION ( 'draft international standard', 'automotive_design', 1998, #18573 ) ;
#5270 = CARTESIAN_POINT ( 'NONE',  ( 231.2217848218749339, -32.57812499938548001, 97.61286128772489690 ) ) ;
#5271 = CARTESIAN_POINT ( 'NONE',  ( 233.9782151781249411, -32.80312499938548143, -47.61286128772501769 ) ) ;
#5272 = CARTESIAN_POINT ( 'NONE',  ( -79.64356964374999848, -32.61562499938548854, 99.99999999999998579 ) ) ;
#5273 = ORIENTED_EDGE ( 'NONE', *, *, #12360, .F. ) ;
#5274 = CARTESIAN_POINT ( 'NONE',  ( -79.64356964375001269, -32.65312499938548285, -98.40857419181659793 ) ) ;
#5275 = LINE ( 'NONE', #14623, #17545 ) ;
#5276 = VERTEX_POINT ( 'NONE', #10120 ) ;
#5277 = CARTESIAN_POINT ( 'NONE',  ( 85.15643035625001289, -34.34062499938548285, 101.5914258081833879 ) ) ;
#5278 = CARTESIAN_POINT ( 'NONE',  ( -85.40000000000000568, -34.48124999877096997, -101.7320508075688679 ) ) ;
#5279 = AXIS2_PLACEMENT_3D ( 'NONE', #5360, #19024, #7006 ) ;
#5280 = CARTESIAN_POINT ( 'NONE',  ( 85.40000000000000568, -34.50000000000000000, 99.99999999999998579 ) ) ;
#5281 = CARTESIAN_POINT ( 'NONE',  ( -79.60045861139941792, -35.00000000000000000, 99.68825842090977574 ) ) ;
#5282 = CARTESIAN_POINT ( 'NONE',  ( -79.39999999999999147, -31.10624999877097352, 101.7320508075688537 ) ) ;
#5283 = CARTESIAN_POINT ( 'NONE',  ( -82.39999999999999147, -34.78124999877096712, 103.4641016151377499 ) ) ;
#5284 = PLANE ( 'NONE',  #17254 ) ;
#5285 = DIRECTION ( 'NONE',  ( 0.000000000000000000, 1.000000000000000000, 0.000000000000000000 ) ) ;
#5286 = CARTESIAN_POINT ( 'NONE',  ( 230.5523683116323355, -32.00000000000000000, 101.8452947671440540 ) ) ;
#5287 = CARTESIAN_POINT ( 'NONE',  ( 235.3564303562499447, -33.06562499938547717, 99.99999999999998579 ) ) ;
#5288 = ORIENTED_EDGE ( 'NONE', *, *, #4451, .T. ) ;
#5289 = CARTESIAN_POINT ( 'NONE',  ( 84.28136653320188998, -32.00000000000000000, -97.98546077809228905 ) ) ;
#5290 =( NAMED_UNIT ( * ) SI_UNIT ( $, .STERADIAN. ) SOLID_ANGLE_UNIT ( ) );
#5291 = CARTESIAN_POINT ( 'NONE',  ( 244.7999999999999545, -32.00000000000000000, -100.0000000000000000 ) ) ;
#5292 = CARTESIAN_POINT ( 'NONE',  ( 229.5999999999999375, -31.78124999877096357, -51.73205080756898866 ) ) ;
#5293 = ORIENTED_EDGE ( 'NONE', *, *, #16453, .F. ) ;
#5294 = CARTESIAN_POINT ( 'NONE',  ( 82.39999999999999147, -32.58749999999999858, 96.99999999999998579 ) ) ;
#5295 = CARTESIAN_POINT ( 'NONE',  ( -79.64356964374998427, -32.20312499938548711, 101.5914258081833879 ) ) ;
#5296 = CARTESIAN_POINT ( 'NONE',  ( -2.805705207896067144, 3.226868319750155312, -3.503898532754364581 ) ) ;
#5297 = ORIENTED_EDGE ( 'NONE', *, *, #16809, .T. ) ;
#5298 = CARTESIAN_POINT ( 'NONE',  ( -82.40000000000001990, -33.88124999877096855, -97.00000000000000000 ) ) ;
#5299 = EDGE_CURVE ( 'NONE', #13270, #4516, #12883, .T. ) ;
#5300 = CARTESIAN_POINT ( 'NONE',  ( 231.0999999999999375, -33.16874999877095576, 97.40192378864668399 ) ) ;
#5301 = ORIENTED_EDGE ( 'NONE', *, *, #430, .F. ) ;
#5302 =( BOUNDED_CURVE ( )  B_SPLINE_CURVE ( 2, ( #5294, #11337, #15740, #17302, #2346, #5391, #3908, #9975, #2531 ),
 .UNSPECIFIED., .F., .F. ) 
 B_SPLINE_CURVE_WITH_KNOTS ( ( 3, 2, 2, 2, 3 ),
 ( 0.4791666666666666297, 0.4861111111111111049, 0.5000000000000000000, 0.5138888888888888395, 0.5208333333333333703 ),
 .UNSPECIFIED. ) 
 CURVE ( )  GEOMETRIC_REPRESENTATION_ITEM ( )  RATIONAL_B_SPLINE_CURVE ( ( 0.9330127018922194093, 0.9330127018922190762, 1.000000000000000000, 0.8660254037844387076, 1.000000000000000000, 0.8660254037844387076, 1.000000000000000000, 0.9330127018922187432, 0.9330127018922192983 ) ) 
 REPRESENTATION_ITEM ( '' )  );
#5303 = CARTESIAN_POINT ( 'NONE',  ( 99.99999999999997158, -5.200000000000008171, -100.0000000000000000 ) ) ;
#5304 = CARTESIAN_POINT ( 'NONE',  ( 82.39999999999999147, -33.48750000000000426, -103.4641016151377499 ) ) ;
#5305 = PLANE ( 'NONE',  #8608 ) ;
#5306 = EDGE_CURVE ( 'NONE', #7789, #13728, #57, .T. ) ;
#5307 = EDGE_CURVE ( 'NONE', #2832, #15250, #5144, .T. ) ;
#5308 = CARTESIAN_POINT ( 'NONE',  ( -79.64356964375001269, -31.41562499938548569, 101.5914258081833879 ) ) ;
#5309 = CARTESIAN_POINT ( 'NONE',  ( -85.40000000000000568, -30.41249999999999787, 101.7320508075688679 ) ) ;
#5310 = UNCERTAINTY_MEASURE_WITH_UNIT (LENGTH_MEASURE( 1.000000000000000082E-05 ), #9085, 'distance_accuracy_value', 'NONE');
#5311 = DIRECTION ( 'NONE',  ( 0.000000000000000000, -1.000000000000000000, 0.000000000000000000 ) ) ;
#5312 = CARTESIAN_POINT ( 'NONE',  ( -99.99999999999998579, 0.000000000000000000, -150.0000000000000000 ) ) ;
#5313 = CARTESIAN_POINT ( 'NONE',  ( 79.77811200999867935, -34.99999999999999289, -100.8506536761476156 ) ) ;
#5314 = CARTESIAN_POINT ( 'NONE',  ( -81.59615242270662350, -33.46740381056766722, 102.9999999999999716 ) ) ;
#5315 = CARTESIAN_POINT ( 'NONE',  ( -79.64356964375001269, -32.57812499938548001, 98.40857419181659793 ) ) ;
#5316 = FACE_OUTER_BOUND ( 'NONE', #1775, .T. ) ;
#5317 = VERTEX_POINT ( 'NONE', #11960 ) ;
#5318 = CARTESIAN_POINT ( 'NONE',  ( 234.0999999999999375, -33.89999999999999147, -47.40192378864679768 ) ) ;
#5319 =( NAMED_UNIT ( * ) PLANE_ANGLE_UNIT ( ) SI_UNIT ( $, .RADIAN. ) );
#5320 = EDGE_CURVE ( 'NONE', #11379, #15041, #19205, .T. ) ;
#5321 = LINE ( 'NONE', #14378, #9896 ) ;
#5322 = CARTESIAN_POINT ( 'NONE',  ( 235.3564303562499447, -33.17812499938548143, 99.99999999999998579 ) ) ;
#5323 = CARTESIAN_POINT ( 'NONE',  ( -85.15643035625001289, -32.95312499938548711, 99.99999999999998579 ) ) ;
#5324 = EDGE_CURVE ( 'NONE', #15108, #13408, #19306, .T. ) ;
#5325 = CARTESIAN_POINT ( 'NONE',  ( 229.8435696437499871, -30.55312499938547788, -48.40857419181671162 ) ) ;
#5326 = EDGE_CURVE ( 'NONE', #11820, #7197, #14994, .T. ) ;
#5327 = ORIENTED_EDGE ( 'NONE', *, *, #12139, .T. ) ;
#5328 = CARTESIAN_POINT ( 'NONE',  ( -2.378468515890074563E-15, 2.859595677584338080, -2.047034997319574945 ) ) ;
#5329 = CARTESIAN_POINT ( 'NONE',  ( -79.64356964375001269, -33.55312499938548854, 101.5914258081833879 ) ) ;
#5330 = CARTESIAN_POINT ( 'NONE',  ( 80.52691934816499497, -34.99999999999999289, 97.94626448418664211 ) ) ;
#5331 = CARTESIAN_POINT ( 'NONE',  ( 81.02178482187500208, -31.34062499938548996, 97.61286128772489690 ) ) ;
#5332 = DIRECTION ( 'NONE',  ( -1.000000000000000000, 0.000000000000000000, 0.000000000000000000 ) ) ;
#5333 = CARTESIAN_POINT ( 'NONE',  ( 232.5999999999999943, -32.72812499938547859, -46.81714838363331666 ) ) ;
#5334 = ADVANCED_BREP_SHAPE_REPRESENTATION ( '', ( #3164, #10540 ), #11151 ) ;
#5335 =( BOUNDED_CURVE ( )  B_SPLINE_CURVE ( 2, ( #521, #6474, #3726, #811, #17019 ),
 .UNSPECIFIED., .F., .F. ) 
 B_SPLINE_CURVE_WITH_KNOTS ( ( 3, 2, 3 ),
 ( 0.000000000000000000, 0.01388888888888888638, 0.02083333333333331136 ),
 .UNSPECIFIED. ) 
 CURVE ( )  GEOMETRIC_REPRESENTATION_ITEM ( )  RATIONAL_B_SPLINE_CURVE ( ( 1.000000000000000000, 0.8660254037844387076, 1.000000000000000000, 0.9330127018922196314, 0.9330127018922194093 ) ) 
 REPRESENTATION_ITEM ( '' )  );
#5336 = CARTESIAN_POINT ( 'NONE',  ( -83.77821517812500929, -33.77812499938548285, 102.3871387122750889 ) ) ;
#5337 = CARTESIAN_POINT ( 'NONE',  ( -85.15643035625001289, -32.95312499938548711, -99.99999999999998579 ) ) ;
#5338 = CARTESIAN_POINT ( 'NONE',  ( 81.02178482187500208, -33.14062499938548711, 97.61286128772489690 ) ) ;
#5339 = CARTESIAN_POINT ( 'NONE',  ( 82.39999999999999147, -33.06562499938548427, -96.81714838363319586 ) ) ;
#5340 = CARTESIAN_POINT ( 'NONE',  ( 229.8435696437499871, -32.42812499938548143, -51.59142580818350865 ) ) ;
#5341 = CARTESIAN_POINT ( 'NONE',  ( -79.64356964374998427, -32.12812499938548427, 98.40857419181659793 ) ) ;
#5342 = EDGE_LOOP ( 'NONE', ( #10734, #16760, #5634, #16827 ) ) ;
#5343 = CARTESIAN_POINT ( 'NONE',  ( 79.64356964375001269, -31.86562499938548143, 98.40857419181659793 ) ) ;
#5344 = CARTESIAN_POINT ( 'NONE',  ( 235.5999999999999375, -34.21874999877096002, -50.00000000000011369 ) ) ;
#5345 = CARTESIAN_POINT ( 'NONE',  ( -80.90000000000000568, -33.75000000000000000, 97.40192378864668399 ) ) ;
#5346 = LINE ( 'NONE', #15787, #16762 ) ;
#5347 = CARTESIAN_POINT ( 'NONE',  ( -81.02178482187500208, -31.19062499938548427, 97.61286128772489690 ) ) ;
#5348 = CARTESIAN_POINT ( 'NONE',  ( 94.79999999999984084, 0.000000000000000000, -150.0000000000000000 ) ) ;
#5349 = ORIENTED_EDGE ( 'NONE', *, *, #15583, .F. ) ;
#5350 = CARTESIAN_POINT ( 'NONE',  ( -79.39999999999999147, -32.96250000000000568, -98.26794919243113213 ) ) ;
#5351 = CARTESIAN_POINT ( 'NONE',  ( 232.5999999999999375, -34.33124999877097139, -47.00000000000011369 ) ) ;
#5352 = CARTESIAN_POINT ( 'NONE',  ( 229.5999999999999375, -34.04999999999999716, -50.00000000000011369 ) ) ;
#5353 = CARTESIAN_POINT ( 'NONE',  ( 83.20384757729337366, -33.50759618943233420, -103.0000000000000000 ) ) ;
#5354 = CARTESIAN_POINT ( 'NONE',  ( 105.2000000000001307, -29.80000000000002203, 147.7999999999999829 ) ) ;
#5355 = ADVANCED_FACE ( 'NONE', ( #16364 ), #7088, .F. ) ;
#5356 = CARTESIAN_POINT ( 'NONE',  ( -83.20384757729337366, -34.80134618820331127, 103.0000000000000000 ) ) ;
#5357 = CARTESIAN_POINT ( 'NONE',  ( -85.15643035624999868, -30.17812499938548498, 98.40857419181659793 ) ) ;
#5358 = CARTESIAN_POINT ( 'NONE',  ( 83.77821517812500929, -34.71562499938548285, 102.3871387122750889 ) ) ;
#5359 = PLANE ( 'NONE',  #13674 ) ;
#5360 = CARTESIAN_POINT ( 'NONE',  ( 232.5999999999999375, -29.99999999999999645, -50.00000000000011369 ) ) ;
#5361 = CARTESIAN_POINT ( 'NONE',  ( 81.02178482187500208, -31.90312499938548996, -102.3871387122750889 ) ) ;
#5362 = CARTESIAN_POINT ( 'NONE',  ( 79.39999999999999147, -32.83124999877097139, 101.7320508075688963 ) ) ;
#5363 = ORIENTED_EDGE ( 'NONE', *, *, #13804, .F. ) ;
#5364 = CARTESIAN_POINT ( 'NONE',  ( 85.40000000000000568, -31.25624999877096855, 98.26794919243111792 ) ) ;
#5365 = CARTESIAN_POINT ( 'NONE',  ( 235.3564303562499447, -34.11562499938548143, 101.5914258081833879 ) ) ;
#5366 = CARTESIAN_POINT ( 'NONE',  ( 231.2217848218749339, -33.32812499938548001, -47.61286128772501769 ) ) ;
#5367 =( BOUNDED_CURVE ( )  B_SPLINE_CURVE ( 2, ( #5722, #18030, #13326, #14989, #8735, #1518, #1324, #5915, #7468 ),
 .UNSPECIFIED., .F., .F. ) 
 B_SPLINE_CURVE_WITH_KNOTS ( ( 3, 2, 2, 2, 3 ),
 ( 0.6875000000000000000, 0.6944444444444444198, 0.7083333333333333703, 0.7222222222222222099, 0.7291666666666668517 ),
 .UNSPECIFIED. ) 
 CURVE ( )  GEOMETRIC_REPRESENTATION_ITEM ( )  RATIONAL_B_SPLINE_CURVE ( ( 0.9330127018922194093, 0.9330127018922194093, 1.000000000000000000, 0.8660254037844387076, 1.000000000000000000, 0.8660254037844387076, 1.000000000000000000, 0.9330127018922177440, 0.9330127018922194093 ) ) 
 REPRESENTATION_ITEM ( '' )  );
#5368 = CARTESIAN_POINT ( 'NONE',  ( -79.64356964375001269, -32.65312499938548285, 101.5914258081833879 ) ) ;
#5369 = CARTESIAN_POINT ( 'NONE',  ( 229.5999999999999375, -32.66249999999999432, -48.26794919243123161 ) ) ;
#5370 = ORIENTED_EDGE ( 'NONE', *, *, #5299, .F. ) ;
#5371 = CARTESIAN_POINT ( 'NONE',  ( -85.15643035624999868, -30.55312499938548854, -98.40857419181659793 ) ) ;
#5372 = DIRECTION ( 'NONE',  ( -0.000000000000000000, -1.000000000000000000, -0.000000000000000000 ) ) ;
#5373 = ORIENTED_EDGE ( 'NONE', *, *, #14122, .T. ) ;
#5374 = CARTESIAN_POINT ( 'NONE',  ( 81.02178482187500208, -33.10312499938548569, 102.3871387122750889 ) ) ;
#5375 = CARTESIAN_POINT ( 'NONE',  ( -79.64356964375001269, -31.79062499938548569, -101.5914258081833879 ) ) ;
#5376 = CARTESIAN_POINT ( 'NONE',  ( 79.39999999999999147, -33.82500000000000284, 99.99999999999998579 ) ) ;
#5377 = CARTESIAN_POINT ( 'NONE',  ( 79.39999999999999147, -34.70624999877097139, -101.7320508075688537 ) ) ;
#5378 = CARTESIAN_POINT ( 'NONE',  ( -83.90000000000000568, -31.21874999877097068, 102.5980762113533018 ) ) ;
#5379 = CARTESIAN_POINT ( 'NONE',  ( -81.02178482187500208, -31.90312499938548996, 102.3871387122750889 ) ) ;
#5380 = CARTESIAN_POINT ( 'NONE',  ( -81.02178482187500208, -32.24062499938548854, -97.61286128772489690 ) ) ;
#5381 = VECTOR ( 'NONE', #10112, 1000.000000000000000 ) ;
#5382 = VECTOR ( 'NONE', #15745, 1000.000000000000000 ) ;
#5383 = CARTESIAN_POINT ( 'NONE',  ( 231.0999999999999375, -32.32499999999999574, -52.59807621135342970 ) ) ;
#5384 = PLANE ( 'NONE',  #12556 ) ;
#5385 = CARTESIAN_POINT ( 'NONE',  ( 232.5999999999999375, -30.11249999999999716, 96.53589838486223584 ) ) ;
#5386 = ORIENTED_EDGE ( 'NONE', *, *, #10187, .T. ) ;
#5387 = CARTESIAN_POINT ( 'NONE',  ( 81.02178482187500208, -33.44062499938548427, -97.61286128772489690 ) ) ;
#5388 = CARTESIAN_POINT ( 'NONE',  ( 229.5999999999999375, -32.60624999877096997, 101.7320508075688679 ) ) ;
#5389 = CARTESIAN_POINT ( 'NONE',  ( 229.5999999999999375, -32.19374999877096144, -50.00000000000011369 ) ) ;
#5390 = ORIENTED_EDGE ( 'NONE', *, *, #10777, .F. ) ;
#5391 = CARTESIAN_POINT ( 'NONE',  ( 85.40000000000000568, -32.73750000000000426, 101.7320508075688821 ) ) ;
#5392 = ADVANCED_FACE ( 'NONE', ( #16075 ), #8994, .T. ) ;
#5393 = CARTESIAN_POINT ( 'NONE',  ( -79.64356964374999848, -31.26562499938548356, 99.99999999999998579 ) ) ;
#5394 = CARTESIAN_POINT ( 'NONE',  ( -3.511755186886750479, 2.826662030176366081, -3.597382984111578086 ) ) ;
#5395 = ORIENTED_EDGE ( 'NONE', *, *, #18087, .T. ) ;
#5396 = CARTESIAN_POINT ( 'NONE',  ( 111.0000000000000000, 6.932050807568741924, -134.9680512646005184 ) ) ;
#5397 = VECTOR ( 'NONE', #15463, 1000.000000000000000 ) ;
#5398 = VECTOR ( 'NONE', #3253, 1000.000000000000000 ) ;
#5399 = CARTESIAN_POINT ( 'NONE',  ( 231.7961524227065695, -33.00134618820329990, 103.0000000000000000 ) ) ;
#5400 = ORIENTED_EDGE ( 'NONE', *, *, #7252, .T. ) ;
#5401 = CARTESIAN_POINT ( 'NONE',  ( -79.39999999999997726, -32.01330983656956164, -100.5399455202751966 ) ) ;
#5402 = B_SPLINE_CURVE_WITH_KNOTS ( 'NONE', 3,
 ( #15422, #3498, #6347, #16796, #13664 ),
 .UNSPECIFIED., .F., .F.,
 ( 4, 1, 4 ),
 ( 3.224213076541126624E-34, 0.002020725942163690940, 0.004041451884327381880 ),
 .UNSPECIFIED. ) ;
#5403 = CARTESIAN_POINT ( 'NONE',  ( 83.90000000000000568, -33.22500000000000142, -97.40192378864668399 ) ) ;
#5404 = CARTESIAN_POINT ( 'NONE',  ( 79.68596062386910717, -31.99999999999998579, -101.2782762865714972 ) ) ;
#5405 = CARTESIAN_POINT ( 'NONE',  ( -85.15643035624999868, -32.54062499938548569, 98.40857419181659793 ) ) ;
#5406 = CARTESIAN_POINT ( 'NONE',  ( -82.39999999999999147, -30.78750000000000497, 103.4641016151377499 ) ) ;
#5407 = CARTESIAN_POINT ( 'NONE',  ( -81.59615242270665192, -34.81740381056767575, -97.00000000000000000 ) ) ;
#5408 = DIRECTION ( 'NONE',  ( -1.000000000000000000, 9.941108744852765039E-17, 0.000000000000000000 ) ) ;
#5409 = CARTESIAN_POINT ( 'NONE',  ( 83.90000000000000568, -34.06874999877096855, 102.5980762113533018 ) ) ;
#5410 = DIRECTION ( 'NONE',  ( -1.000000000000000000, -0.000000000000000000, 0.000000000000000000 ) ) ;
#5411 = CARTESIAN_POINT ( 'NONE',  ( 85.32499745258149915, -34.99999999999999289, 100.1587029275220857 ) ) ;
#5412 = AXIS2_PLACEMENT_3D ( 'NONE', #12997, #10448, #13381 ) ;
#5413 = CARTESIAN_POINT ( 'NONE',  ( -84.28136653320150629, -32.00000000000001421, -102.0145392219080378 ) ) ;
#5414 = VERTEX_POINT ( 'NONE', #2974 ) ;
#5415 = CARTESIAN_POINT ( 'NONE',  ( 80.90000000000000568, -32.85000000000000142, 102.5980762113533018 ) ) ;
#5416 = DIRECTION ( 'NONE',  ( 0.000000000000000000, -1.000000000000000000, 0.000000000000000000 ) ) ;
#5417 = EDGE_CURVE ( 'NONE', #7672, #16645, #2784, .T. ) ;
#5418 = DIRECTION ( 'NONE',  ( 0.000000000000000000, 0.000000000000000000, 1.000000000000000000 ) ) ;
#5419 =( BOUNDED_CURVE ( )  B_SPLINE_CURVE ( 2, ( #12902, #18869, #17206, #3529, #9483, #3810, #8120 ),
 .UNSPECIFIED., .F., .F. ) 
 B_SPLINE_CURVE_WITH_KNOTS ( ( 3, 2, 2, 3 ),
 ( 0.3702305174531529963, 0.3750000000000000000, 0.3888888888888888951, 0.3958333333333334259 ),
 .UNSPECIFIED. ) 
 CURVE ( )  GEOMETRIC_REPRESENTATION_ITEM ( )  RATIONAL_B_SPLINE_CURVE ( ( 0.9395835397632832375, 0.9539927561172885095, 1.000000000000000000, 0.8660254037844387076, 1.000000000000000000, 0.9330127018922185211, 0.9330127018922192983 ) ) 
 REPRESENTATION_ITEM ( '' )  );
#5420 = CARTESIAN_POINT ( 'NONE',  ( 231.2217848218749339, -34.22812499938548569, 102.3871387122750889 ) ) ;
#5421 = CARTESIAN_POINT ( 'NONE',  ( -82.39999999999999147, -34.19062499938548427, 103.1828516163667899 ) ) ;
#5422 = CARTESIAN_POINT ( 'NONE',  ( 229.8435696437499303, -30.59062499938547575, -50.00000000000011369 ) ) ;
#5423 = ORIENTED_EDGE ( 'NONE', *, *, #9703, .T. ) ;
#5424 = CARTESIAN_POINT ( 'NONE',  ( -80.07894310789832559, -34.99999999999998579, -98.50261820439553162 ) ) ;
#5425 = CARTESIAN_POINT ( 'NONE',  ( -81.02178482187500208, -33.44062499938548427, 97.61286128772489690 ) ) ;
#5426 = VECTOR ( 'NONE', #9102, 999.9999999999998863 ) ;
#5427 =( BOUNDED_CURVE ( )  B_SPLINE_CURVE ( 2, ( #18561, #13959, #15330, #9670, #16706, #9469, #15631, #12593, #601 ),
 .UNSPECIFIED., .F., .F. ) 
 B_SPLINE_CURVE_WITH_KNOTS ( ( 3, 2, 2, 2, 3 ),
 ( 0.3541666666666666852, 0.3611111111111111049, 0.3750000000000000000, 0.3888888888888888951, 0.3958333333333334259 ),
 .UNSPECIFIED. ) 
 CURVE ( )  GEOMETRIC_REPRESENTATION_ITEM ( )  RATIONAL_B_SPLINE_CURVE ( ( 0.9330127018922194093, 0.9330127018922196314, 1.000000000000000000, 0.8660254037844387076, 1.000000000000000000, 0.8660254037844387076, 1.000000000000000000, 0.9330127018922185211, 0.9330127018922192983 ) ) 
 REPRESENTATION_ITEM ( '' )  );
#5428 = CARTESIAN_POINT ( 'NONE',  ( 83.20384757729338787, -32.10134618820330132, -102.9999999999999858 ) ) ;
#5429 = CARTESIAN_POINT ( 'NONE',  ( 85.15643035624999868, -31.45312499938548356, 98.40857419181659793 ) ) ;
#5430 = CARTESIAN_POINT ( 'NONE',  ( 244.7999999999999545, -32.00000000000002842, 147.7999999999999829 ) ) ;
#5431 = EDGE_CURVE ( 'NONE', #16462, #15718, #14014, .T. ) ;
#5432 = CARTESIAN_POINT ( 'NONE',  ( 235.3564303562499447, -32.16562499938547859, -50.00000000000011369 ) ) ;
#5433 = CARTESIAN_POINT ( 'NONE',  ( -81.02178482187500208, -34.45312499938548711, 97.61286128772489690 ) ) ;
#5434 = CARTESIAN_POINT ( 'NONE',  ( -79.64356964374998427, -34.49062499938548854, -101.5914258081833879 ) ) ;
#5435 = CARTESIAN_POINT ( 'NONE',  ( 79.64356964375001269, -32.57812499938548001, 101.5914258081833879 ) ) ;
#5436 = CARTESIAN_POINT ( 'NONE',  ( 81.02178482187500208, -34.90312499938548285, -97.61286128772489690 ) ) ;
#5437 = CARTESIAN_POINT ( 'NONE',  ( 232.5999999999999375, -33.17812499938548143, -46.81714838363331666 ) ) ;
#5438 = CARTESIAN_POINT ( 'NONE',  ( -83.77821517812500929, -33.81562499938548427, 97.61286128772489690 ) ) ;
#5439 = CARTESIAN_POINT ( 'NONE',  ( 81.02178482187500208, -31.19062499938548427, -97.61286128772489690 ) ) ;
#5440 = ADVANCED_FACE ( 'NONE', ( #12445 ), #16746, .F. ) ;
#5441 = VERTEX_POINT ( 'NONE', #16943 ) ;
#5442 = DIRECTION ( 'NONE',  ( -2.775557561562891351E-15, -1.000000000000000000, 0.000000000000000000 ) ) ;
#5443 = CARTESIAN_POINT ( 'NONE',  ( 234.0999999999999375, -34.29374999877096286, -47.40192378864679768 ) ) ;
#5444 = CARTESIAN_POINT ( 'NONE',  ( -80.90000000000000568, -34.64999999999999858, 97.40192378864668399 ) ) ;
#5445 = CARTESIAN_POINT ( 'NONE',  ( -85.15643035625001289, -33.29062499938547859, 99.99999999999998579 ) ) ;
#5446 = CARTESIAN_POINT ( 'NONE',  ( -79.64356964375001269, -30.40312499938548285, 101.5914258081833879 ) ) ;
#5447 = CARTESIAN_POINT ( 'NONE',  ( -82.39999999999999147, -31.23750000000000071, 102.9999999999999858 ) ) ;
#5448 = CARTESIAN_POINT ( 'NONE',  ( -85.03799702444352704, -32.00000000000000000, 99.18121545504318703 ) ) ;
#5450 = CARTESIAN_POINT ( 'NONE',  ( 229.8435696437499303, -32.84062499938547575, 99.99999999999998579 ) ) ;
#5449 =( BOUNDED_SURFACE ( )  B_SPLINE_SURFACE ( 3, 2, ( 
 ( #10219, #14318, #11297 ),
 ( #5546, #11395, #17358 ),
 ( #9833, #14605, #8551 ),
 ( #3967, #9933, #7095 ),
 ( #17264, #16185, #17550 ),
 ( #15891, #2497, #7188 ) ),
 .UNSPECIFIED., .F., .F., .F. ) 
 B_SPLINE_SURFACE_WITH_KNOTS ( ( 4, 2, 4 ),
 ( 3, 3 ),
 ( 0.01651999345535504551, 0.01858032176739834312, 0.02064065007944163727 ),
 ( 0.000000000000000000, 1.000000000000000000 ),
 .UNSPECIFIED. ) 
 GEOMETRIC_REPRESENTATION_ITEM ( )  RATIONAL_B_SPLINE_SURFACE ( (
 ( 1.000000000000000000, 0.8047781103519391355, 1.000000000000000000),
 ( 1.000000000000000000, 0.8123785825602164445, 1.000000000000000000),
 ( 1.000000000000000000, 0.8190671539791195555, 1.000000000000000000),
 ( 1.000000000000000000, 0.8192352254831950509, 1.000000000000000000),
 ( 1.000000000000000000, 0.8126129677213795865, 1.000000000000000000),
 ( 1.000000000000000000, 0.8047712537969733404, 1.000000000000000000) ) ) 
 REPRESENTATION_ITEM ( '' )  SURFACE ( )  );
#5451 = CARTESIAN_POINT ( 'NONE',  ( 231.7961524227065695, -33.95759618943232283, -47.00000000000011369 ) ) ;
#5452 = CARTESIAN_POINT ( 'NONE',  ( -80.90000000000000568, -31.04606250001229029, 97.40192378864668399 ) ) ;
#5453 = EDGE_CURVE ( 'NONE', #8145, #9264, #12430, .T. ) ;
#5454 = CARTESIAN_POINT ( 'NONE',  ( -82.40000000000000568, -30.00000000000000355, 99.99999999999998579 ) ) ;
#5455 = CARTESIAN_POINT ( 'NONE',  ( -81.59615242270665192, -32.77634618820330559, 97.00000000000000000 ) ) ;
#5456 = CARTESIAN_POINT ( 'NONE',  ( 233.4038475772933054, -33.01740381056766438, 103.0000000000000142 ) ) ;
#5457 = CARTESIAN_POINT ( 'NONE',  ( 230.4677467024383191, -31.99999999999999289, 98.24409948398863435 ) ) ;
#5458 = CARTESIAN_POINT ( 'NONE',  ( 3.999999999999999112, -1.539600717839012978, -3.300726591567080703 ) ) ;
#5459 = CARTESIAN_POINT ( 'NONE',  ( 0.1217565302851127407, -3.710888496608923948, 0.5725525826504677118 ) ) ;
#5460 = CARTESIAN_POINT ( 'NONE',  ( -79.68596062386970402, -32.00000000000002132, -98.72172371342720965 ) ) ;
#5461 = CARTESIAN_POINT ( 'NONE',  ( 83.77821517812500929, -34.82812499938548711, -97.61286128772489690 ) ) ;
#5462 = CARTESIAN_POINT ( 'NONE',  ( 232.5999999999999375, -33.93749999999999289, 103.0000000000000000 ) ) ;
#5463 = VERTEX_POINT ( 'NONE', #4647 ) ;
#5464 = CARTESIAN_POINT ( 'NONE',  ( 83.90000000000000568, -33.61874999877097281, 102.5980762113533018 ) ) ;
#5465 = CARTESIAN_POINT ( 'NONE',  ( 235.3564303562499447, -34.94062499938547717, 98.40857419181659793 ) ) ;
#5466 = CARTESIAN_POINT ( 'NONE',  ( 229.8435696437499303, -32.05312499938548143, -50.00000000000011369 ) ) ;
#5467 = CARTESIAN_POINT ( 'NONE',  ( 4.071447262713890680, -4.041451884327388555, 0.000000000000000000 ) ) ;
#5468 = ORIENTED_EDGE ( 'NONE', *, *, #13152, .T. ) ;
#5469 = EDGE_CURVE ( 'NONE', #14354, #3376, #4936, .T. ) ;
#5470 = CARTESIAN_POINT ( 'NONE',  ( -81.02178482187500208, -32.09062499938548285, -102.3871387122750889 ) ) ;
#5471 = CARTESIAN_POINT ( 'NONE',  ( -82.40000000000000568, -30.00000000000000355, 96.99999999999998579 ) ) ;
#5472 = ORIENTED_EDGE ( 'NONE', *, *, #2325, .T. ) ;
#5473 = CARTESIAN_POINT ( 'NONE',  ( 85.15643035625001289, -33.81562499938548427, 98.40857419181659793 ) ) ;
#5474 = CARTESIAN_POINT ( 'NONE',  ( -81.02178482187500208, -31.75312499938548427, -102.3871387122750889 ) ) ;
#5475 = CARTESIAN_POINT ( 'NONE',  ( 83.90000000000000568, -33.22500000000000142, 102.5980762113533018 ) ) ;
#5476 = CARTESIAN_POINT ( 'NONE',  ( -82.40000000000000568, -34.38749999999999574, 102.9999999999999858 ) ) ;
#5477 = CARTESIAN_POINT ( 'NONE',  ( -85.40000000000000568, -35.34374999877096712, 99.99999999999998579 ) ) ;
#5478 = CARTESIAN_POINT ( 'NONE',  ( -83.77821517812500929, -31.22812499938548569, 97.61286128772489690 ) ) ;
#5479 = CARTESIAN_POINT ( 'NONE',  ( -79.64356964374998427, -33.47812499938547859, -101.5914258081833879 ) ) ;
#5480 = VECTOR ( 'NONE', #10167, 1000.000000000000000 ) ;
#5481 = CARTESIAN_POINT ( 'NONE',  ( 230.4285530052381716, -35.00000000000000000, 97.92073041325133431 ) ) ;
#5482 = CARTESIAN_POINT ( 'NONE',  ( 80.90000000000000568, -31.59374999877097423, -102.5980762113533018 ) ) ;
#5483 = CARTESIAN_POINT ( 'NONE',  ( 235.5999999999999943, -31.53749999999999432, 98.26794919243110371 ) ) ;
#5484 =( BOUNDED_CURVE ( )  B_SPLINE_CURVE ( 2, ( #2285, #14199, #3945, #5522, #10104, #17437, #5432, #15962, #2664, #17143, #1027, #17529, #8342, #6798, #6889, #933, #8625, #14578, #17336, #12744, #7171, #5333, #14298, #9911, #4048, #19091, #5712, #3748, #9715, #8249, #1602, #8825, #4631, #10484, #10297, #13217, #14979, #8916, #7263, #45, #2961, #4526, #11851, #10584, #14877, #19188, #5805, #16258, #16160, #11756, #18019, #14679, #13415, #1506, #7457, #2866, #7643, #17727, #8726, #19291, #5996, #7360, #14781, #10196, #1314, #6096, #16350, #4337, #11948, #17625, #15072, #17918, #7549, #5905, #16447, #13599, #9019, #10389, #3148, #2771, #16549, #1407, #239 ),
 .UNSPECIFIED., .F., .F. ) 
 B_SPLINE_CURVE_WITH_KNOTS ( ( 3, 2, 2, 2, 2, 2, 2, 2, 2, 2, 2, 2, 2, 2, 2, 2, 2, 2, 2, 2, 2, 2, 2, 2, 2, 2, 2, 2, 2, 2, 2, 2, 2, 2, 2, 2, 2, 2, 2, 2, 2, 3 ),
 ( 0.3716916592826016719, 0.3750191855951751085, 0.3900199530189821240, 0.4050207204427891394, 0.4200214878665962104, 0.4350222552904032258, 0.4500230227142102413, 0.4650237901380172567, 0.4800245575618242166, 0.4950253249856312321, 0.5100260924094381920, 0.5250268598332452630, 0.5400276272570523339, 0.5550283946808592939, 0.5700291621046663648, 0.5850299295284733248, 0.6000306969522803957, 0.6150314643760873556, 0.6300322317998944266, 0.6450329992237013865, 0.6600337666475084575, 0.6750345340713154174, 0.6900353014951223773, 0.7050360689189294483, 0.7200368363427364082, 0.7350376037665435902, 0.7500383711903504391, 0.7650391386141575101, 0.7800399060379645810, 0.7950406734617716520, 0.8100414408855785009, 0.8250422083093855719, 0.8400429757331926428, 0.8550437431569996027, 0.8700445105808065627, 0.8850452780046136336, 0.9000460454284207046, 0.9150468128522275535, 0.9300475802760346244, 0.9450483476998416954, 0.9600491151236485443, 0.9717223562348840105 ),
 .UNSPECIFIED. ) 
 CURVE ( )  GEOMETRIC_REPRESENTATION_ITEM ( )  RATIONAL_B_SPLINE_CURVE ( ( 0.9537471549767071455, 0.9702812541832913640, 1.000000000000000000, 0.8660254037844387076, 1.000000000000000000, 0.8660254037844387076, 1.000000000000000000, 0.8660254037844387076, 1.000000000000000000, 0.8660254037844387076, 1.000000000000000000, 0.8660254037844387076, 1.000000000000000000, 0.8660254037844387076, 1.000000000000000000, 0.8660254037844387076, 1.000000000000000000, 0.8660254037844387076, 1.000000000000000000, 0.8660254037844387076, 1.000000000000000000, 0.8660254037844387076, 1.000000000000000000, 0.8660254037844387076, 1.000000000000000000, 0.8660254037844387076, 1.000000000000000000, 0.8660254037844387076, 1.000000000000000000, 0.8660254037844387076, 1.000000000000000000, 0.8660254037844387076, 1.000000000000000000, 0.8660254037844387076, 1.000000000000000000, 0.8660254037844387076, 1.000000000000000000, 0.8660254037844387076, 1.000000000000000000, 0.8660254037844387076, 1.000000000000000000, 0.8660254037844387076, 1.000000000000000000, 0.8660254037844387076, 1.000000000000000000, 0.8660254037844387076, 1.000000000000000000, 0.8660254037844387076, 1.000000000000000000, 0.8660254037844387076, 1.000000000000000000, 0.8660254037844387076, 1.000000000000000000, 0.8660254037844387076, 1.000000000000000000, 0.8660254037844387076, 1.000000000000000000, 0.8660254037844387076, 1.000000000000000000, 0.8660254037844387076, 1.000000000000000000, 0.8660254037844387076, 1.000000000000000000, 0.8660254037844387076, 1.000000000000000000, 0.8660254037844387076, 1.000000000000000000, 0.8660254037844387076, 1.000000000000000000, 0.8660254037844387076, 1.000000000000000000, 0.8660254037844387076, 1.000000000000000000, 0.8660254037844387076, 1.000000000000000000, 0.8660254037844387076, 1.000000000000000000, 0.8660254037844387076, 1.000000000000000000, 0.8660254037844387076, 1.000000000000000000, 0.8957441496011311344, 0.9537471549767251311 ) ) 
 REPRESENTATION_ITEM ( '' )  );
#5485 = VERTEX_POINT ( 'NONE', #3555 ) ;
#5486 = CARTESIAN_POINT ( 'NONE',  ( 81.02178482187500208, -34.04062499938548569, -102.3871387122750889 ) ) ;
#5487 = SURFACE_STYLE_FILL_AREA ( #15543 ) ;
#5488 = CARTESIAN_POINT ( 'NONE',  ( 232.5999999999999375, -32.08124999877095718, 103.4641016151377499 ) ) ;
#5489 = DIRECTION ( 'NONE',  ( 0.000000000000000000, -0.5000000000000012212, -0.8660254037844380415 ) ) ;
#5490 = CARTESIAN_POINT ( 'NONE',  ( -79.64356964374999848, -32.16562499938548569, 99.99999999999998579 ) ) ;
#5491 = VERTEX_POINT ( 'NONE', #9512 ) ;
#5492 = ORIENTED_EDGE ( 'NONE', *, *, #5896, .T. ) ;
#5493 = CARTESIAN_POINT ( 'NONE',  ( 3.972066048304732533, -2.740530939476237826, 2.384802634787742903 ) ) ;
#5494 = AXIS2_PLACEMENT_3D ( 'NONE', #4448, #17749, #2884 ) ;
#5495 = CARTESIAN_POINT ( 'NONE',  ( 232.5999999999999375, -33.65624999877096002, -53.00000000000011369 ) ) ;
#5496 = VERTEX_POINT ( 'NONE', #18223 ) ;
#5497 = CARTESIAN_POINT ( 'NONE',  ( 4.175813232069148562, -2.061359961916374495, -3.570380186727398097 ) ) ;
#5498 = CARTESIAN_POINT ( 'NONE',  ( 79.39999999999999147, -32.47500000000000142, -99.99999999999998579 ) ) ;
#5499 = CARTESIAN_POINT ( 'NONE',  ( -82.40000000000000568, -30.00000000000000355, 99.99999999999998579 ) ) ;
#5500 = CARTESIAN_POINT ( 'NONE',  ( -79.64356964374999848, -32.27812499938548996, 99.99999999999998579 ) ) ;
#5501 = CARTESIAN_POINT ( 'NONE',  ( -83.90000000000000568, -33.22500000000000142, 97.40192378864668399 ) ) ;
#5502 = DIRECTION ( 'NONE',  ( -0.000000000000000000, -1.000000000000000000, -0.000000000000000000 ) ) ;
#5503 = CARTESIAN_POINT ( 'NONE',  ( -82.40000000000000568, -30.00000000000000355, 99.99999999999998579 ) ) ;
#5504 = CARTESIAN_POINT ( 'NONE',  ( 117.5000000000000142, 12.69999999999998508, 110.0000000000000142 ) ) ;
#5505 = DIRECTION ( 'NONE',  ( 0.000000000000000000, 1.000000000000000000, 0.000000000000000000 ) ) ;
#5506 = CARTESIAN_POINT ( 'NONE',  ( -85.15643035625001289, -35.09062499938548285, 99.99999999999998579 ) ) ;
#5507 = AXIS2_PLACEMENT_3D ( 'NONE', #11122, #6741, #6844 ) ;
#5508 = FACE_OUTER_BOUND ( 'NONE', #8430, .T. ) ;
#5509 = ORIENTED_EDGE ( 'NONE', *, *, #9593, .T. ) ;
#5510 = CARTESIAN_POINT ( 'NONE',  ( 231.6691923799541826, -35.05289549976082952, -53.55789078125459923 ) ) ;
#5511 = DIRECTION ( 'NONE',  ( 0.000000000000000000, 0.000000000000000000, -1.000000000000000000 ) ) ;
#5512 = LINE ( 'NONE', #4130, #5853 ) ;
#5513 = CARTESIAN_POINT ( 'NONE',  ( 0.000000000000000000, 0.000000000000000000, 150.0000000000000000 ) ) ;
#5514 = CARTESIAN_POINT ( 'NONE',  ( -85.15643035625001289, -33.85312499938549280, 99.99999999999998579 ) ) ;
#5515 = CARTESIAN_POINT ( 'NONE',  ( 232.5999999999999375, -30.47812499938547859, -46.81714838363331666 ) ) ;
#5516 = EDGE_LOOP ( 'NONE', ( #2348, #4717, #11356, #462 ) ) ;
#5517 = CARTESIAN_POINT ( 'NONE',  ( -79.64356964375001269, -34.37812499938548427, 98.40857419181659793 ) ) ;
#5518 = AXIS2_PLACEMENT_3D ( 'NONE', #5499, #7330, #4208 ) ;
#5519 = CARTESIAN_POINT ( 'NONE',  ( 83.90000000000000568, -32.26874999877097139, -97.40192378864668399 ) ) ;
#5520 = CARTESIAN_POINT ( 'NONE',  ( 79.64356964374999848, -34.41562499938548569, 99.99999999999998579 ) ) ;
#5521 = CARTESIAN_POINT ( 'NONE',  ( -82.39999999999999147, -32.81250000000000000, 97.00000000000000000 ) ) ;
#5522 = CARTESIAN_POINT ( 'NONE',  ( 232.5999999999999943, -32.05312499938548143, -53.18285161636690361 ) ) ;
#5523 = CARTESIAN_POINT ( 'NONE',  ( -81.02178482187500208, -33.25312499938548427, 102.3871387122750889 ) ) ;
#5524 = CARTESIAN_POINT ( 'NONE',  ( -82.39999999999999147, -34.64062499938548711, -96.81714838363319586 ) ) ;
#5525 = CARTESIAN_POINT ( 'NONE',  ( 79.64356964375001269, -33.02812499938548285, 101.5914258081833879 ) ) ;
#5526 = CARTESIAN_POINT ( 'NONE',  ( 81.02178482187500208, -33.25312499938548427, -102.3871387122750889 ) ) ;
#5527 = CARTESIAN_POINT ( 'NONE',  ( 229.8435696437499303, -32.84062499938547575, -50.00000000000011369 ) ) ;
#5528 = CARTESIAN_POINT ( 'NONE',  ( -82.39999999999999147, -32.27812499938548285, 103.1828516163667899 ) ) ;
#5529 = CARTESIAN_POINT ( 'NONE',  ( 83.77821517812500929, -31.86562499938548498, -102.3871387122750889 ) ) ;
#5530 = VERTEX_POINT ( 'NONE', #6109 ) ;
#5531 = CARTESIAN_POINT ( 'NONE',  ( 113.0000000000000000, 10.19999999999997264, -145.0000000000000000 ) ) ;
#5532 = CARTESIAN_POINT ( 'NONE',  ( 232.5999999999999659, -32.58749999999999858, -47.00000000000011369 ) ) ;
#5533 = CARTESIAN_POINT ( 'NONE',  ( -79.39999999999999147, -34.31250000000000000, 101.7320508075688537 ) ) ;
#5534 =( BOUNDED_CURVE ( )  B_SPLINE_CURVE ( 2, ( #5351, #14315, #7972, #17062, #2012, #14029, #15698, #15501, #2209 ),
 .UNSPECIFIED., .F., .F. ) 
 B_SPLINE_CURVE_WITH_KNOTS ( ( 3, 2, 2, 2, 3 ),
 ( 0.7291666666666665186, 0.7361111111111111605, 0.7500000000000000000, 0.7638888888888888395, 0.7708333333333332593 ),
 .UNSPECIFIED. ) 
 CURVE ( )  GEOMETRIC_REPRESENTATION_ITEM ( )  RATIONAL_B_SPLINE_CURVE ( ( 0.9330127018922194093, 0.9330127018922177440, 1.000000000000000000, 0.8660254037844387076, 1.000000000000000000, 0.8660254037844387076, 1.000000000000000000, 0.9330127018922198534, 0.9330127018922192983 ) ) 
 REPRESENTATION_ITEM ( '' )  );
#5535 = CARTESIAN_POINT ( 'NONE',  ( -82.39999999999999147, -33.17812499938548854, 103.1828516163667899 ) ) ;
#5536 = CARTESIAN_POINT ( 'NONE',  ( -81.02178482187500208, -31.64062499938548356, 97.61286128772489690 ) ) ;
#5537 = ADVANCED_BREP_SHAPE_REPRESENTATION ( '', ( #3102, #10540 ), #13638 ) ;
#5538 = ORIENTED_EDGE ( 'NONE', *, *, #13776, .F. ) ;
#5539 = FACE_OUTER_BOUND ( 'NONE', #11115, .T. ) ;
#5540 = VECTOR ( 'NONE', #11167, 1000.000000000000000 ) ;
#5541 = EDGE_CURVE ( 'NONE', #6725, #3433, #7696, .T. ) ;
#5542 = CARTESIAN_POINT ( 'NONE',  ( 233.9782151781249411, -33.44062499938547717, 97.61286128772489690 ) ) ;
#5543 = CARTESIAN_POINT ( 'NONE',  ( 82.40000000000001990, -32.53124999877097423, -103.0000000000000000 ) ) ;
#5544 = CARTESIAN_POINT ( 'NONE',  ( -80.90000000000000568, -31.19606250001229242, 102.5980762113533018 ) ) ;
#5545 = ADVANCED_FACE ( 'NONE', ( #5770 ), #11721, .T. ) ;
#5546 = CARTESIAN_POINT ( 'NONE',  ( 3.961551342853556257, 3.742715940867794355, -0.5174258321190280396 ) ) ;
#5547 = CARTESIAN_POINT ( 'NONE',  ( 82.40000000000000568, -30.00000000000000355, -99.99999999999998579 ) ) ;
#5548 = CARTESIAN_POINT ( 'NONE',  ( -82.39999999999999147, -30.47812499938548569, 103.1828516163667899 ) ) ;
#5549 = CARTESIAN_POINT ( 'NONE',  ( 99.99999999999997158, -34.99999999999999289, -100.0000000000000000 ) ) ;
#5550 = LINE ( 'NONE', #17172, #6198 ) ;
#5551 = CARTESIAN_POINT ( 'NONE',  ( 82.40000000000001990, -34.55624999877097281, -97.00000000000000000 ) ) ;
#5552 = DIRECTION ( 'NONE',  ( -0.000000000000000000, -1.000000000000000000, -0.000000000000000000 ) ) ;
#5553 = CARTESIAN_POINT ( 'NONE',  ( 83.77821517812500929, -33.32812499938548711, -102.3871387122750889 ) ) ;
#5554 = CARTESIAN_POINT ( 'NONE',  ( 82.39999999999999147, -32.98124999877096286, 96.99999999999998579 ) ) ;
#5555 = EDGE_LOOP ( 'NONE', ( #2903, #16505, #8121, #701, #10451 ) ) ;
#5556 = CARTESIAN_POINT ( 'NONE',  ( 79.39999999999999147, -33.28124999877096712, 101.7320508075688821 ) ) ;
#5557 = CARTESIAN_POINT ( 'NONE',  ( 233.9782151781249411, -34.00312499938547717, 97.61286128772489690 ) ) ;
#5558 = CARTESIAN_POINT ( 'NONE',  ( 231.2217848218749339, -32.42812499938548143, -47.61286128772501769 ) ) ;
#5559 = AXIS2_PLACEMENT_3D ( 'NONE', #9062, #8681, #10434 ) ;
#5560 =( GEOMETRIC_REPRESENTATION_CONTEXT ( 3 ) GLOBAL_UNCERTAINTY_ASSIGNED_CONTEXT ( ( #13232 ) ) GLOBAL_UNIT_ASSIGNED_CONTEXT ( ( #17901, #1486, #2645 ) ) REPRESENTATION_CONTEXT ( 'NONE', 'WORKASPACE' ) );
#5561 = EDGE_CURVE ( 'NONE', #7994, #6852, #15867, .T. ) ;
#5562 = CARTESIAN_POINT ( 'NONE',  ( 0.000000000000000000, 3.061616997868383634E-16, -2.500000000000000444 ) ) ;
#5563 = CARTESIAN_POINT ( 'NONE',  ( 83.90000000000000568, -34.12500000000000000, 102.5980762113533018 ) ) ;
#5564 = VERTEX_POINT ( 'NONE', #18707 ) ;
#5565 = CARTESIAN_POINT ( 'NONE',  ( -81.02178482187500208, -33.59062499938548285, -97.61286128772489690 ) ) ;
#5566 = EDGE_CURVE ( 'NONE', #1546, #13533, #6780, .T. ) ;
#5567 = LINE ( 'NONE', #5471, #2553 ) ;
#5568 = VERTEX_POINT ( 'NONE', #832 ) ;
#5569 = CARTESIAN_POINT ( 'NONE',  ( 231.0999999999999375, -33.67499999999999716, -52.59807621135342970 ) ) ;
#5570 = AXIS2_PLACEMENT_3D ( 'NONE', #17281, #9661, #12969 ) ;
#5571 = CARTESIAN_POINT ( 'NONE',  ( -82.39999999999999147, -30.59062499938548640, -96.81714838363319586 ) ) ;
#5572 = CARTESIAN_POINT ( 'NONE',  ( 79.39999999999999147, -34.72500000000000142, 99.99999999999998579 ) ) ;
#5573 = CARTESIAN_POINT ( 'NONE',  ( 235.3564303562499447, -30.47812499938547859, 99.99999999999998579 ) ) ;
#5574 = CARTESIAN_POINT ( 'NONE',  ( -80.90000000000000568, -30.54768749875868039, 97.40192378864668399 ) ) ;
#5575 = CARTESIAN_POINT ( 'NONE',  ( -81.02178482187500208, -30.55312499938548854, 102.3871387122750889 ) ) ;
#5576 = CARTESIAN_POINT ( 'NONE',  ( -81.02178482187500208, -32.09062499938548285, -102.3871387122750889 ) ) ;
#5577 = CIRCLE ( 'NONE', #1508, 9.999999999999998224 ) ;
#5578 = CARTESIAN_POINT ( 'NONE',  ( 232.6775203606193543, -35.00000000000000711, 102.7610832838413728 ) ) ;
#5579 = CARTESIAN_POINT ( 'NONE',  ( 83.90000000000000568, -32.26874999877097139, -97.40192378864668399 ) ) ;
#5580 = CARTESIAN_POINT ( 'NONE',  ( 231.0999999999999375, -32.17499999999999716, 102.5980762113533018 ) ) ;
#5581 = ORIENTED_EDGE ( 'NONE', *, *, #18310, .T. ) ;
#5582 = DIRECTION ( 'NONE',  ( 1.000000000000000000, -1.586032892321652285E-15, 0.000000000000000000 ) ) ;
#5583 = FILL_AREA_STYLE_COLOUR ( '', #9554 ) ;
#5584 = CARTESIAN_POINT ( 'NONE',  ( 229.5999999999999375, -33.13124999877096144, 98.26794919243111792 ) ) ;
#5585 = PLANE ( 'NONE',  #17400 ) ;
#5586 = CARTESIAN_POINT ( 'NONE',  ( -80.90000000000000568, -35.19374999877096855, 102.5980762113533018 ) ) ;
#5587 = CARTESIAN_POINT ( 'NONE',  ( -79.64356964374998427, -31.75312499938548427, 101.5914258081833879 ) ) ;
#5588 = VERTEX_POINT ( 'NONE', #3652 ) ;
#5589 = ORIENTED_EDGE ( 'NONE', *, *, #18015, .T. ) ;
#5590 = CARTESIAN_POINT ( 'NONE',  ( -82.40000000000001990, -34.16250000000000853, -103.0000000000000000 ) ) ;
#5591 = CONICAL_SURFACE ( 'NONE', #11501, 5.560781378645573980, 1.221730476396046816 ) ;
#5592 = CARTESIAN_POINT ( 'NONE',  ( 4.204015924366189871, -1.626724848190933548, -3.610627190413393084 ) ) ;
#5593 = VERTEX_POINT ( 'NONE', #3938 ) ;
#5594 = LINE ( 'NONE', #5303, #17269 ) ;
#5595 = CARTESIAN_POINT ( 'NONE',  ( 82.39999999999999147, -32.36250000000000426, -96.53589838486223584 ) ) ;
#5596 = EDGE_CURVE ( 'NONE', #8302, #8568, #9710, .T. ) ;
#5597 = CARTESIAN_POINT ( 'NONE',  ( 0.03027795055833725976, 0.6888063905328605241, 3.500000000000000444 ) ) ;
#5598 = CARTESIAN_POINT ( 'NONE',  ( -79.64356964375001269, -31.79062499938548569, 98.40857419181659793 ) ) ;
#5599 = CARTESIAN_POINT ( 'NONE',  ( -85.40000000000000568, -30.93750000000000355, 98.26794919243111792 ) ) ;
#5600 = CARTESIAN_POINT ( 'NONE',  ( 234.6787480663869587, -35.00000000000000000, -52.02344717699244825 ) ) ;
#5601 = CARTESIAN_POINT ( 'NONE',  ( 244.7999999999999545, -29.80000000000000782, -100.0000000000000000 ) ) ;
#5602 = DIRECTION ( 'NONE',  ( 0.000000000000000000, 0.000000000000000000, 1.000000000000000000 ) ) ;
#5603 = EDGE_CURVE ( 'NONE', #14525, #15327, #14680, .T. ) ;
#5604 = CARTESIAN_POINT ( 'NONE',  ( -4.000000000000000000, -2.309401076758512694, -3.433295621305382461 ) ) ;
#5605 = CARTESIAN_POINT ( 'NONE',  ( -81.02178482187500208, -34.79062499938548569, 97.61286128772489690 ) ) ;
#5606 = CARTESIAN_POINT ( 'NONE',  ( -94.79999999999999716, -3.000000000000000000, -150.0000000000000000 ) ) ;
#5607 = VERTEX_POINT ( 'NONE', #19156 ) ;
#5608 = CARTESIAN_POINT ( 'NONE',  ( -81.02178482187500208, -31.34062499938548996, -97.61286128772489690 ) ) ;
#5609 = CARTESIAN_POINT ( 'NONE',  ( 234.1461053235294116, -35.00000000000001421, 97.51091559654268792 ) ) ;
#5610 = CARTESIAN_POINT ( 'NONE',  ( 82.65333140691207348, -34.99995246259152992, 102.9892844631211943 ) ) ;
#5611 = CARTESIAN_POINT ( 'NONE',  ( 233.9782151781249411, -34.15312499938547575, 102.3871387122750889 ) ) ;
#5612 = CARTESIAN_POINT ( 'NONE',  ( -82.39999999999999147, -34.64062499938548711, 103.1828516163667899 ) ) ;
#5613 = CYLINDRICAL_SURFACE ( 'NONE', #11292, 3.000000000000002665 ) ;
#5614 = CARTESIAN_POINT ( 'NONE',  ( 232.5999999999999375, -34.64062499938548001, -46.81714838363331666 ) ) ;
#5615 = ORIENTED_EDGE ( 'NONE', *, *, #11611, .F. ) ;
#5616 = CARTESIAN_POINT ( 'NONE',  ( -81.02178482187500208, -34.79062499938548569, 97.61286128772489690 ) ) ;
#5617 = CARTESIAN_POINT ( 'NONE',  ( -79.39999999999999147, -33.82500000000000284, -99.99999999999998579 ) ) ;
#5618 = CARTESIAN_POINT ( 'NONE',  ( 85.40000000000000568, -30.03750000000000497, 101.7320508075688679 ) ) ;
#5619 = CARTESIAN_POINT ( 'NONE',  ( -82.40000000000001990, -34.55624999877097281, -103.0000000000000000 ) ) ;
#5620 = CARTESIAN_POINT ( 'NONE',  ( 229.8435696437499303, -30.59062499938547575, 99.99999999999998579 ) ) ;
#5621 = CARTESIAN_POINT ( 'NONE',  ( -85.15643035625001289, -33.81562499938548427, 101.5914258081833879 ) ) ;
#5622 = CARTESIAN_POINT ( 'NONE',  ( -82.39999999999999147, -33.74062499938548854, -96.81714838363319586 ) ) ;
#5623 = CARTESIAN_POINT ( 'NONE',  ( 85.15643035624999868, -33.70312499938548711, 98.40857419181659793 ) ) ;
#5624 = CARTESIAN_POINT ( 'NONE',  ( 82.39999999999999147, -33.51562499938548001, -96.81714838363319586 ) ) ;
#5625 = CARTESIAN_POINT ( 'NONE',  ( 232.5999999999999375, -31.01249999999999218, -53.46410161513786363 ) ) ;
#5626 = CARTESIAN_POINT ( 'NONE',  ( -82.39999999999999147, -33.62812499938548427, 103.1828516163667899 ) ) ;
#5627 = CARTESIAN_POINT ( 'NONE',  ( 79.64356964375001269, -30.85312499938548569, -101.5914258081833879 ) ) ;
#5628 = ORIENTED_EDGE ( 'NONE', *, *, #3556, .F. ) ;
#5629 = CARTESIAN_POINT ( 'NONE',  ( 82.39999999999999147, -33.96562499938548285, 103.1828516163667899 ) ) ;
#5630 = CARTESIAN_POINT ( 'NONE',  ( 4.071447262713887127, -2.020725942163688060, 3.500000000000000444 ) ) ;
#5631 = CARTESIAN_POINT ( 'NONE',  ( -83.90000000000000568, -33.67500000000000426, 97.40192378864668399 ) ) ;
#5632 = CARTESIAN_POINT ( 'NONE',  ( -85.15643035625001289, -32.39062499938548711, 99.99999999999998579 ) ) ;
#5633 = CARTESIAN_POINT ( 'NONE',  ( -79.64356964375001269, -30.77812499938548285, 98.40857419181659793 ) ) ;
#5634 = ORIENTED_EDGE ( 'NONE', *, *, #8204, .T. ) ;
#5635 = DIRECTION ( 'NONE',  ( 1.000000000000000000, 0.000000000000000000, 0.000000000000000000 ) ) ;
#5636 = FACE_OUTER_BOUND ( 'NONE', #4016, .T. ) ;
#5637 = CARTESIAN_POINT ( 'NONE',  ( 80.85389467647095785, -35.00000000000000000, -97.51091559654246055 ) ) ;
#5638 = DIRECTION ( 'NONE',  ( -0.000000000000000000, -1.000000000000000000, -0.000000000000000000 ) ) ;
#5639 = CARTESIAN_POINT ( 'NONE',  ( 1.411581201560190495E-15, 4.862606272033091592, -3.745885042887436622 ) ) ;
#5640 = DIRECTION ( 'NONE',  ( -1.000000000000000000, 0.000000000000000000, 0.000000000000000000 ) ) ;
#5641 = FACE_OUTER_BOUND ( 'NONE', #4086, .T. ) ;
#5642 = CARTESIAN_POINT ( 'NONE',  ( -83.90000000000000568, -33.67500000000000426, 97.40192378864668399 ) ) ;
#5643 = CARTESIAN_POINT ( 'NONE',  ( 79.64356964374999848, -33.17812499938548854, 99.99999999999998579 ) ) ;
#5644 = DIRECTION ( 'NONE',  ( 0.000000000000000000, -1.000000000000000000, 0.000000000000000000 ) ) ;
#5645 = CARTESIAN_POINT ( 'NONE',  ( -83.20384757729337366, -32.55134618820330417, -97.00000000000000000 ) ) ;
#5646 = CARTESIAN_POINT ( 'NONE',  ( 85.15643035625001289, -32.95312499938548711, -99.99999999999998579 ) ) ;
#5647 = LINE ( 'NONE', #8277, #1494 ) ;
#5648 =( BOUNDED_CURVE ( )  B_SPLINE_CURVE ( 2, ( #963, #5645, #8461, #7103, #17557, #4074, #17463, #1052, #11591 ),
 .UNSPECIFIED., .F., .F. ) 
 B_SPLINE_CURVE_WITH_KNOTS ( ( 3, 2, 2, 2, 3 ),
 ( 0.3958333333333334259, 0.4027777777777777901, 0.4166666666666666852, 0.4305555555555555802, 0.4374999999999999445 ),
 .UNSPECIFIED. ) 
 CURVE ( )  GEOMETRIC_REPRESENTATION_ITEM ( )  RATIONAL_B_SPLINE_CURVE ( ( 0.9330127018922192983, 0.9330127018922200755, 1.000000000000000000, 0.8660254037844387076, 1.000000000000000000, 0.8660254037844387076, 1.000000000000000000, 0.9330127018922198534, 0.9330127018922192983 ) ) 
 REPRESENTATION_ITEM ( '' )  );
#5649 = VERTEX_POINT ( 'NONE', #17689 ) ;
#5650 = CARTESIAN_POINT ( 'NONE',  ( 83.90000000000000568, -33.16874999877096286, 102.5980762113533018 ) ) ;
#5651 = CARTESIAN_POINT ( 'NONE',  ( 231.2217848218749339, -34.67812499938548143, 102.3871387122750889 ) ) ;
#5652 = CARTESIAN_POINT ( 'NONE',  ( 231.2217848218749339, -34.67812499938548143, -47.61286128772501769 ) ) ;
#5653 = ADVANCED_FACE ( 'NONE', ( #4303 ), #18139, .F. ) ;
#5654 = EDGE_CURVE ( 'NONE', #8815, #6725, #2269, .T. ) ;
#5655 = CARTESIAN_POINT ( 'NONE',  ( -85.15643035624999868, -35.05312499938548143, 101.5914258081833879 ) ) ;
#5656 = FACE_OUTER_BOUND ( 'NONE', #14229, .T. ) ;
#5657 = ORIENTED_EDGE ( 'NONE', *, *, #6752, .F. ) ;
#5658 = CARTESIAN_POINT ( 'NONE',  ( -79.64356964374999848, -34.41562499938548569, -99.99999999999998579 ) ) ;
#5659 = CARTESIAN_POINT ( 'NONE',  ( 82.40000000000001990, -33.26250000000000284, 103.0000000000000000 ) ) ;
#5660 = ORIENTED_EDGE ( 'NONE', *, *, #12059, .T. ) ;
#5661 = FACE_OUTER_BOUND ( 'NONE', #15170, .T. ) ;
#5662 = CARTESIAN_POINT ( 'NONE',  ( -79.39999999999999147, -35.11874999877096570, -99.99999999999998579 ) ) ;
#5663 = CARTESIAN_POINT ( 'NONE',  ( -79.39999999999999147, -32.41874999877096997, -99.99999999999998579 ) ) ;
#5664 = CARTESIAN_POINT ( 'NONE',  ( -85.40000000000000568, -34.50000000000000000, 99.99999999999998579 ) ) ;
#5665 = CARTESIAN_POINT ( 'NONE',  ( -80.90000000000000568, -34.59374999877096712, 97.40192378864668399 ) ) ;
#5666 = CARTESIAN_POINT ( 'NONE',  ( -82.39999999999999147, -32.16562499938549280, 96.81714838363319586 ) ) ;
#5667 = EDGE_CURVE ( 'NONE', #16293, #11985, #4795, .T. ) ;
#5668 = CARTESIAN_POINT ( 'NONE',  ( -83.77821517812500929, -32.46562499938548285, -102.3871387122750889 ) ) ;
#5669 = ADVANCED_FACE ( 'NONE', ( #7615 ), #6793, .F. ) ;
#5670 = CARTESIAN_POINT ( 'NONE',  ( 234.8201511961208610, -35.00000000000002842, 101.6434491389464085 ) ) ;
#5671 = CARTESIAN_POINT ( 'NONE',  ( 85.40000000000000568, -32.64374999877097139, -99.99999999999998579 ) ) ;
#5672 = CARTESIAN_POINT ( 'NONE',  ( 235.5999999999999375, -30.67499999999999361, 99.99999999999998579 ) ) ;
#5673 = EDGE_LOOP ( 'NONE', ( #17275, #17497, #6927, #13 ) ) ;
#5674 = LINE ( 'NONE', #17681, #6647 ) ;
#5675 =( NAMED_UNIT ( * ) SI_UNIT ( $, .STERADIAN. ) SOLID_ANGLE_UNIT ( ) );
#5676 = CARTESIAN_POINT ( 'NONE',  ( 235.5999999999999943, -32.00624999877096144, 101.7320508075688537 ) ) ;
#5677 = CARTESIAN_POINT ( 'NONE',  ( 235.5999999999999375, -31.51874999877096073, -50.00000000000011369 ) ) ;
#5678 = ADVANCED_FACE ( 'NONE', ( #3214, #1752, #7519 ), #10551, .F. ) ;
#5679 = PLANE ( 'NONE',  #11770 ) ;
#5680 = CARTESIAN_POINT ( 'NONE',  ( -85.15643035625001289, -31.94062499938548427, 99.99999999999998579 ) ) ;
#5681 = VERTEX_POINT ( 'NONE', #7710 ) ;
#5682 = EDGE_LOOP ( 'NONE', ( #18585, #1968, #18788, #8286, #10927 ) ) ;
#5683 = CARTESIAN_POINT ( 'NONE',  ( 111.0000000000000000, 10.19999999999997620, -137.3499999999999943 ) ) ;
#5684 = ORIENTED_EDGE ( 'NONE', *, *, #2906, .F. ) ;
#5685 = CARTESIAN_POINT ( 'NONE',  ( 79.39999999999999147, -33.41250000000000142, -101.7320508075688537 ) ) ;
#5686 = CARTESIAN_POINT ( 'NONE',  ( 80.80636817121802551, -31.99999999999999289, -102.4696265554868120 ) ) ;
#5687 = CARTESIAN_POINT ( 'NONE',  ( -79.64356964374999848, -31.37812499938548427, 99.99999999999998579 ) ) ;
#5688 = CARTESIAN_POINT ( 'NONE',  ( -79.39999999999999147, -31.12500000000000355, 99.99999999999998579 ) ) ;
#5689 = DIRECTION ( 'NONE',  ( 0.000000000000000000, 0.000000000000000000, -1.000000000000000000 ) ) ;
#5690 = CARTESIAN_POINT ( 'NONE',  ( -84.69814150944628750, -35.26302329524826007, 98.07164691963323833 ) ) ;
#5691 = CARTESIAN_POINT ( 'NONE',  ( 96.99999999999994316, -29.80000000000000426, 150.0000000000000000 ) ) ;
#5692 = DIRECTION ( 'NONE',  ( 1.000000000000000000, 0.000000000000000000, 0.000000000000000000 ) ) ;
#5693 = EDGE_LOOP ( 'NONE', ( #573, #12918, #11844, #8837 ) ) ;
#5694 = CARTESIAN_POINT ( 'NONE',  ( -82.39999999999999147, -32.05312499938548854, -103.1828516163667899 ) ) ;
#5695 = DIRECTION ( 'NONE',  ( 0.000000000000000000, 0.000000000000000000, -1.000000000000000000 ) ) ;
#5696 = AXIS2_PLACEMENT_3D ( 'NONE', #18059, #9146, #15110 ) ;
#5697 = DIRECTION ( 'NONE',  ( -0.000000000000000000, -1.000000000000000000, -0.000000000000000000 ) ) ;
#5698 = CARTESIAN_POINT ( 'NONE',  ( 233.9782151781249411, -34.45312499938548001, 97.61286128772489690 ) ) ;
#5699 = CARTESIAN_POINT ( 'NONE',  ( -81.02178482187500208, -31.64062499938548356, 97.61286128772489690 ) ) ;
#5700 = CARTESIAN_POINT ( 'NONE',  ( -83.20384757729337366, -34.14240381056766438, 97.00000000000000000 ) ) ;
#5701 = CARTESIAN_POINT ( 'NONE',  ( 229.8435696437499871, -33.32812499938548001, -51.59142580818350865 ) ) ;
#5702 = ORIENTED_EDGE ( 'NONE', *, *, #11394, .F. ) ;
#5703 = ORIENTED_EDGE ( 'NONE', *, *, #17732, .T. ) ;
#5704 = ADVANCED_FACE ( 'NONE', ( #7325 ), #4400, .F. ) ;
#5705 = CARTESIAN_POINT ( 'NONE',  ( -81.02178482187500208, -34.34062499938548285, 97.61286128772489690 ) ) ;
#5706 = CARTESIAN_POINT ( 'NONE',  ( -84.42750213138106119, -35.00000000000000711, -102.2200415044235768 ) ) ;
#5708 = CARTESIAN_POINT ( 'NONE',  ( 82.39999999999999147, -34.30312499938548143, 103.1828516163667899 ) ) ;
#5707 = APPLICATION_CONTEXT ( 'automotive_design' ) ;
#5709 = CARTESIAN_POINT ( 'NONE',  ( -83.20384757729337366, -32.79240381056766296, 97.00000000000000000 ) ) ;
#5711 = CARTESIAN_POINT ( 'NONE',  ( 235.3564303562499447, -32.57812499938547290, 98.40857419181659793 ) ) ;
#5710=STYLED_ITEM('',(#19371),#7579);
#5712 = CARTESIAN_POINT ( 'NONE',  ( 231.2217848218749339, -32.91562499938547148, -52.38713871227520968 ) ) ;
#5713 = FACE_OUTER_BOUND ( 'NONE', #17639, .T. ) ;
#5714 = CARTESIAN_POINT ( 'NONE',  ( 85.40000000000000568, -33.09374999877096712, -99.99999999999998579 ) ) ;
#5715 = CARTESIAN_POINT ( 'NONE',  ( 82.39999999999999147, -32.50312499938548427, -96.81714838363319586 ) ) ;
#5716 = CARTESIAN_POINT ( 'NONE',  ( 231.0999999999999375, -31.42499999999999361, -52.59807621135342970 ) ) ;
#5717 = CARTESIAN_POINT ( 'NONE',  ( -81.02178482187500208, -32.99062499938548854, 97.61286128772489690 ) ) ;
#5718 = CARTESIAN_POINT ( 'NONE',  ( 82.39999999999999147, -31.37812499938548427, -103.1828516163667899 ) ) ;
#5719 = VERTEX_POINT ( 'NONE', #10355 ) ;
#5720 = EDGE_CURVE ( 'NONE', #10587, #11600, #18768, .T. ) ;
#5721 = CARTESIAN_POINT ( 'NONE',  ( 85.15643035624999868, -34.71562499938548285, 98.40857419181659793 ) ) ;
#5722 = CARTESIAN_POINT ( 'NONE',  ( 82.40000000000000568, -33.71249999999998437, -96.99999999999998579 ) ) ;
#5723 = CARTESIAN_POINT ( 'NONE',  ( 229.8435696437499303, -30.70312499938548001, -50.00000000000011369 ) ) ;
#5724 = AXIS2_PLACEMENT_3D ( 'NONE', #18737, #1139, #15893 ) ;
#5725 = CARTESIAN_POINT ( 'NONE',  ( -83.77821517812500929, -32.46562499938548285, 97.61286128772489690 ) ) ;
#5726 = ORIENTED_EDGE ( 'NONE', *, *, #18216, .T. ) ;
#5727 = CARTESIAN_POINT ( 'NONE',  ( 2.500000000000000888, 3.061616997868384127E-16, -4.974599999999998801 ) ) ;
#5728 = CARTESIAN_POINT ( 'NONE',  ( 235.3564303562499447, -33.47812499938547859, 98.40857419181659793 ) ) ;
#5729 = CARTESIAN_POINT ( 'NONE',  ( 79.73531137350353504, -34.99999999999998579, -98.99456257074372445 ) ) ;
#5730 = CARTESIAN_POINT ( 'NONE',  ( -80.90000000000000568, -31.49606250001229313, 97.40192378864668399 ) ) ;
#5731 = CARTESIAN_POINT ( 'NONE',  ( -82.40000000000000568, -34.61250000000001137, 97.00000000000000000 ) ) ;
#5732 = CARTESIAN_POINT ( 'NONE',  ( 231.2583267490322783, -32.00000000000000000, -47.53412486788969460 ) ) ;
#5733 = CARTESIAN_POINT ( 'NONE',  ( -85.15643035624999868, -31.00312499938548072, 101.5914258081833879 ) ) ;
#5734 = CARTESIAN_POINT ( 'NONE',  ( -82.40000000000000568, -30.00000000000000355, 99.99999999999998579 ) ) ;
#5735 = CARTESIAN_POINT ( 'NONE',  ( 79.64356964374999848, -32.27812499938548996, 99.99999999999998579 ) ) ;
#5736 = DIRECTION ( 'NONE',  ( -0.000000000000000000, 0.000000000000000000, 1.000000000000000000 ) ) ;
#5737 = CARTESIAN_POINT ( 'NONE',  ( 85.15643035624999868, -33.36562499938548854, -101.5914258081833879 ) ) ;
#5738 = CARTESIAN_POINT ( 'NONE',  ( -82.39999999999999147, -32.39062499938548001, -96.81714838363319586 ) ) ;
#5739 = ORIENTED_EDGE ( 'NONE', *, *, #2325, .F. ) ;
#5740 = CARTESIAN_POINT ( 'NONE',  ( 79.39999999999999147, -33.73124999877096997, 101.7320508075688821 ) ) ;
#5741 = CARTESIAN_POINT ( 'NONE',  ( 234.4730806518346924, -35.00000000000004263, -47.94626448418657105 ) ) ;
#5742 = CARTESIAN_POINT ( 'NONE',  ( 82.40000000000001990, -32.75624999877096855, 103.0000000000000000 ) ) ;
#5743 = CARTESIAN_POINT ( 'NONE',  ( 234.0999999999999375, -34.29374999877096286, 102.5980762113533018 ) ) ;
#5744 = CARTESIAN_POINT ( 'NONE',  ( 83.92761994969310990, -32.00000000000000711, 102.3311504458557266 ) ) ;
#5745 = ORIENTED_EDGE ( 'NONE', *, *, #13934, .T. ) ;
#5746 = CARTESIAN_POINT ( 'NONE',  ( -85.15643035624999868, -34.67812499938548143, -101.5914258081833879 ) ) ;
#5747 = CARTESIAN_POINT ( 'NONE',  ( 0.1381419387119273146, -1.355287006778810310, -3.499999999999999556 ) ) ;
#5748 = ORIENTED_EDGE ( 'NONE', *, *, #15939, .F. ) ;
#5749 = CARTESIAN_POINT ( 'NONE',  ( -82.39999999999999147, -32.30624999877096570, 96.99999999999998579 ) ) ;
#5750 = CARTESIAN_POINT ( 'NONE',  ( -85.15643035624999868, -30.66562499938548569, -98.40857419181659793 ) ) ;
#5751 = CARTESIAN_POINT ( 'NONE',  ( -81.90908125315185373, -32.00000000000000000, -102.8381494550067146 ) ) ;
#5752 = CARTESIAN_POINT ( 'NONE',  ( -85.40000000000000568, -31.33124999877096428, -101.7320508075688679 ) ) ;
#5753 = CARTESIAN_POINT ( 'NONE',  ( 233.9782151781249411, -31.45312499938548356, 102.3871387122750889 ) ) ;
#5754 = CARTESIAN_POINT ( 'NONE',  ( -80.90000000000000568, -33.69374999877096855, 97.40192378864668399 ) ) ;
#5755 = CARTESIAN_POINT ( 'NONE',  ( -79.64356964375001269, -32.31562499938548427, 101.5914258081833879 ) ) ;
#5756 = CARTESIAN_POINT ( 'NONE',  ( -85.15643035625001289, -33.70312499938548711, -98.40857419181659793 ) ) ;
#5757 = CARTESIAN_POINT ( 'NONE',  ( 80.90000000000000568, -32.55000000000000426, -102.5980762113533018 ) ) ;
#5758 = CARTESIAN_POINT ( 'NONE',  ( 231.7961524227065695, -32.15759618943231857, -47.00000000000010658 ) ) ;
#5759 = CARTESIAN_POINT ( 'NONE',  ( 82.39999999999999147, -32.75624999877096855, -96.53589838486223584 ) ) ;
#5760 = CARTESIAN_POINT ( 'NONE',  ( 229.5999999999999375, -32.21249999999999858, 101.7320508075688679 ) ) ;
#5761 = ORIENTED_EDGE ( 'NONE', *, *, #908, .T. ) ;
#5762 = CARTESIAN_POINT ( 'NONE',  ( 83.77821517812500929, -34.11562499938548854, -102.3871387122750889 ) ) ;
#5763 = CARTESIAN_POINT ( 'NONE',  ( 232.5999999999999375, -33.65624999877096002, 96.53589838486223584 ) ) ;
#5764 = CARTESIAN_POINT ( 'NONE',  ( 234.0999999999999375, -32.79374999877096286, -52.59807621135342970 ) ) ;
#5765 = CARTESIAN_POINT ( 'NONE',  ( -85.15643035625001289, -33.77812499938548285, 98.40857419181659793 ) ) ;
#5766 = VERTEX_POINT ( 'NONE', #11822 ) ;
#5767 = VERTEX_POINT ( 'NONE', #8883 ) ;
#5768 = DIRECTION ( 'NONE',  ( 1.000000000000000000, -0.000000000000000000, -2.407412430484046130E-31 ) ) ;
#5769 = ADVANCED_FACE ( 'NONE', ( #14842 ), #8101, .T. ) ;
#5770 = FACE_OUTER_BOUND ( 'NONE', #4056, .T. ) ;
#5771 = CARTESIAN_POINT ( 'NONE',  ( 233.4038475772933339, -34.18259618943231715, -53.00000000000011369 ) ) ;
#5772 = EDGE_LOOP ( 'NONE', ( #13611, #15376, #12036, #11824, #17883, #13763, #14671, #14544, #10950, #1539, #4530, #13500, #356, #18146, #2833, #4485, #16249 ) ) ;
#5773 = CARTESIAN_POINT ( 'NONE',  ( -85.40000000000000568, -31.70624999877096784, 101.7320508075688821 ) ) ;
#5774 = FACE_OUTER_BOUND ( 'NONE', #4295, .T. ) ;
#5775 = DIRECTION ( 'NONE',  ( 0.000000000000000000, 0.000000000000000000, 1.000000000000000000 ) ) ;
#5776 = CARTESIAN_POINT ( 'NONE',  ( -83.77821517812500929, -32.87812499938548427, 102.3871387122750889 ) ) ;
#5777 = CARTESIAN_POINT ( 'NONE',  ( -82.39999999999999147, -31.23750000000000071, 103.4641016151377499 ) ) ;
#5778 = FACE_OUTER_BOUND ( 'NONE', #6806, .T. ) ;
#5779 = ADVANCED_FACE ( 'NONE', ( #18461 ), #15526, .T. ) ;
#5780 = DIRECTION ( 'NONE',  ( -1.000000000000000000, 0.000000000000000000, 0.000000000000000000 ) ) ;
#5781 = CARTESIAN_POINT ( 'NONE',  ( -83.77821517812500929, -34.56562499938548427, 102.3871387122750889 ) ) ;
#5782 = CARTESIAN_POINT ( 'NONE',  ( 112.8867513459481984, 10.19999999999997264, -150.0000000000000000 ) ) ;
#5783 = VERTEX_POINT ( 'NONE', #595 ) ;
#5784 = FILL_AREA_STYLE ('',( #17803 ) ) ;
#5785 = CARTESIAN_POINT ( 'NONE',  ( -85.15643035624999868, -35.16562499938547859, -98.40857419181659793 ) ) ;
#5786 = CARTESIAN_POINT ( 'NONE',  ( 232.5999999999999375, -33.43124999877096570, -47.00000000000011369 ) ) ;
#5787 = AXIS2_PLACEMENT_3D ( 'NONE', #12206, #15328, #15237 ) ;
#5788 = CARTESIAN_POINT ( 'NONE',  ( 102.9999999999999858, -5.200000000000008171, 150.0000000000000000 ) ) ;
#5789 = CARTESIAN_POINT ( 'NONE',  ( 235.3564303562499447, -33.62812499938547717, 99.99999999999998579 ) ) ;
#5790 = CARTESIAN_POINT ( 'NONE',  ( -82.39999999999999147, -30.47812499938548569, 103.1828516163667899 ) ) ;
#5791 = CARTESIAN_POINT ( 'NONE',  ( -85.40000000000000568, -34.08749999999999858, 98.26794919243111792 ) ) ;
#5792 = ADVANCED_FACE ( 'NONE', ( #3411 ), #15625, .T. ) ;
#5793 = CARTESIAN_POINT ( 'NONE',  ( 235.3564303562499447, -33.51562499938548001, -50.00000000000011369 ) ) ;
#5795 = EDGE_CURVE ( 'NONE', #12381, #14868, #11628, .T. ) ;
#5794 = VERTEX_POINT ( 'NONE', #1941 ) ;
#5796 = ORIENTED_EDGE ( 'NONE', *, *, #3028, .F. ) ;
#5797 = CARTESIAN_POINT ( 'NONE',  ( -85.39999999999999147, -34.97364041986484295, -101.0919042218176287 ) ) ;
#5798 = CARTESIAN_POINT ( 'NONE',  ( -85.40000000000000568, -31.80000000000000071, 99.99999999999998579 ) ) ;
#5799 = EDGE_CURVE ( 'NONE', #5933, #17663, #13613, .T. ) ;
#5800 = CYLINDRICAL_SURFACE ( 'NONE', #19120, 3.000000000000002665 ) ;
#5801 = CARTESIAN_POINT ( 'NONE',  ( 83.90000000000000568, -30.37500000000000355, 97.40192378864668399 ) ) ;
#5802 = CARTESIAN_POINT ( 'NONE',  ( 82.40000000000001990, -34.16250000000000853, -97.00000000000000000 ) ) ;
#5803 = CARTESIAN_POINT ( 'NONE',  ( 229.8435696437499303, -31.49062499938547788, 99.99999999999998579 ) ) ;
#5804 = AXIS2_PLACEMENT_3D ( 'NONE', #2094, #16854, #8053 ) ;
#5805 = CARTESIAN_POINT ( 'NONE',  ( 231.2217848218749339, -33.66562499938547859, -47.61286128772501769 ) ) ;
#5806 = FACE_OUTER_BOUND ( 'NONE', #783, .T. ) ;
#5807 = CARTESIAN_POINT ( 'NONE',  ( 85.15643035624999868, -34.67812499938548143, 101.5914258081833879 ) ) ;
#5808 = CARTESIAN_POINT ( 'NONE',  ( 82.39999999999999147, -30.25312499938548783, -96.81714838363319586 ) ) ;
#5809 = EDGE_CURVE ( 'NONE', #11864, #5485, #16801, .T. ) ;
#5810 = CARTESIAN_POINT ( 'NONE',  ( 232.5999999999999375, -30.33749999999999503, -46.53589838486234953 ) ) ;
#5811 = CARTESIAN_POINT ( 'NONE',  ( 85.40000000000000568, -34.91250000000000142, -101.7320508075688821 ) ) ;
#5812 = CARTESIAN_POINT ( 'NONE',  ( 79.64356964374999848, -33.96562499938548285, -99.99999999999998579 ) ) ;
#5813 = AXIS2_PLACEMENT_3D ( 'NONE', #1655, #1933, #7894 ) ;
#5814 = ORIENTED_EDGE ( 'NONE', *, *, #8205, .T. ) ;
#5815 = CARTESIAN_POINT ( 'NONE',  ( 79.64356964375001269, -35.01562499938548711, 98.40857419181659793 ) ) ;
#5816 = CARTESIAN_POINT ( 'NONE',  ( 234.0999999999999375, -32.94374999877096144, 102.5980762113533018 ) ) ;
#5817 = CARTESIAN_POINT ( 'NONE',  ( 232.5999999999999375, -31.94062499938548072, -46.81714838363331666 ) ) ;
#5818 = VECTOR ( 'NONE', #10453, 1000.000000000000000 ) ;
#5819 = CARTESIAN_POINT ( 'NONE',  ( -85.15643035625001289, -32.84062499938548285, 99.99999999999998579 ) ) ;
#5820 = VERTEX_POINT ( 'NONE', #9267 ) ;
#5821 = CARTESIAN_POINT ( 'NONE',  ( -84.25709831968909214, -35.00000000000001421, 102.1174602701862000 ) ) ;
#5822 = CARTESIAN_POINT ( 'NONE',  ( 231.2217848218749339, -32.31562499938547717, 102.3871387122750889 ) ) ;
#5823 = CARTESIAN_POINT ( 'NONE',  ( 79.59365286754818669, -35.00000000000000711, -99.92898555286036810 ) ) ;
#5824 = CARTESIAN_POINT ( 'NONE',  ( -83.90000000000000568, -33.22106250001229455, 97.40192378864668399 ) ) ;
#5825 = EDGE_CURVE ( 'NONE', #10334, #6130, #15629, .T. ) ;
#5826 = DIRECTION ( 'NONE',  ( 0.000000000000000000, 2.001604010742465719E-15, -1.000000000000000000 ) ) ;
#5827 = CARTESIAN_POINT ( 'NONE',  ( -81.59615242270660929, -32.32634618820329564, 96.99999999999997158 ) ) ;
#5828 = CARTESIAN_POINT ( 'NONE',  ( -81.02178482187500208, -31.19062499938548427, 97.61286128772489690 ) ) ;
#5829 = CARTESIAN_POINT ( 'NONE',  ( 111.0000000000000000, 10.19999999999997620, -139.9999999999999716 ) ) ;
#5830 = CARTESIAN_POINT ( 'NONE',  ( 85.15643035625001289, -32.95312499938548711, 99.99999999999998579 ) ) ;
#5831 = FACE_OUTER_BOUND ( 'NONE', #12802, .T. ) ;
#5832 = CARTESIAN_POINT ( 'NONE',  ( 231.0999999999999375, -33.22499999999999432, -52.59807621135342970 ) ) ;
#5833 = CARTESIAN_POINT ( 'NONE',  ( 82.39999999999999147, -34.41562499938547859, -96.81714838363319586 ) ) ;
#5834 = CARTESIAN_POINT ( 'NONE',  ( -82.39999999999999147, -31.04062499938548569, -96.81714838363319586 ) ) ;
#5835 = ORIENTED_EDGE ( 'NONE', *, *, #12376, .F. ) ;
#5836 = CARTESIAN_POINT ( 'NONE',  ( 79.39999999999999147, -33.76874999877097139, 99.99999999999998579 ) ) ;
#5837 = ITEM_DEFINED_TRANSFORMATION ( 'NONE', 'NONE', #2688,  #10540 ) ;
#5838 = FACE_OUTER_BOUND ( 'NONE', #10290, .T. ) ;
#5839 = CARTESIAN_POINT ( 'NONE',  ( 231.7961524227065979, -34.85759618943232852, -47.00000000000011369 ) ) ;
#5840 = CARTESIAN_POINT ( 'NONE',  ( -83.77821517812500929, -31.52812499938548996, 102.3871387122750889 ) ) ;
#5841 = CARTESIAN_POINT ( 'NONE',  ( 80.24181665645362216, -31.99999999999999289, 102.0230471654357700 ) ) ;
#5842 = ORIENTED_EDGE ( 'NONE', *, *, #8076, .F. ) ;
#5843 = CARTESIAN_POINT ( 'NONE',  ( -83.77821517812500929, -34.56562499938548427, -97.61286128772489690 ) ) ;
#5844 = AXIS2_PLACEMENT_3D ( 'NONE', #3295, #7601, #17779 ) ;
#5845 = DIRECTION ( 'NONE',  ( -1.000000000000000000, -0.000000000000000000, -0.000000000000000000 ) ) ;
#5846 = ORIENTED_EDGE ( 'NONE', *, *, #4830, .F. ) ;
#5847 = CARTESIAN_POINT ( 'NONE',  ( 232.5999999999999375, -33.48749999999999716, -47.00000000000011369 ) ) ;
#5848 = CARTESIAN_POINT ( 'NONE',  ( -83.77821517812500929, -32.42812499938548854, -97.61286128772489690 ) ) ;
#5849 = CARTESIAN_POINT ( 'NONE',  ( -80.60346964438549833, -31.99999999999999289, -102.3251727584376312 ) ) ;
#5850 = CARTESIAN_POINT ( 'NONE',  ( -85.40000000000000568, -32.19374999877096855, -99.99999999999998579 ) ) ;
#5851 = CARTESIAN_POINT ( 'NONE',  ( 235.3564303562499447, -32.69062499938547717, 98.40857419181659793 ) ) ;
#5852 = CARTESIAN_POINT ( 'NONE',  ( -83.90000000000000568, -32.27268749875867115, 97.40192378864668399 ) ) ;
#5853 = VECTOR ( 'NONE', #8425, 1000.000000000000000 ) ;
#5854 = CARTESIAN_POINT ( 'NONE',  ( -85.15643035625001289, -33.40312499938548285, 99.99999999999998579 ) ) ;
#5855 = CARTESIAN_POINT ( 'NONE',  ( -85.40000000000000568, -33.54374999877096286, 99.99999999999998579 ) ) ;
#5856 = CARTESIAN_POINT ( 'NONE',  ( -4.197393957002303999, -7.773935952363655451E-14, -3.503767560748929810 ) ) ;
#5857 = LINE ( 'NONE', #6051, #9262 ) ;
#5858 = CARTESIAN_POINT ( 'NONE',  ( 85.40000000000000568, -32.15624999877096712, -101.7320508075688679 ) ) ;
#5859 = VECTOR ( 'NONE', #11257, 1000.000000000000000 ) ;
#5860 = CARTESIAN_POINT ( 'NONE',  ( 231.0999999999999375, -34.57499999999999574, 97.40192378864668399 ) ) ;
#5861 = VERTEX_POINT ( 'NONE', #12682 ) ;
#5862 = CARTESIAN_POINT ( 'NONE',  ( 234.0999999999999375, -34.59374999877096002, 97.40192378864668399 ) ) ;
#5863 = CARTESIAN_POINT ( 'NONE',  ( 0.000000000000000000, 0.000000000000000000, 0.000000000000000000 ) ) ;
#5864 = CARTESIAN_POINT ( 'NONE',  ( 229.5999999999999375, -34.40624999877096002, 101.7320508075688679 ) ) ;
#5865 = CARTESIAN_POINT ( 'NONE',  ( 231.0999999999999375, -34.51874999877096428, -52.59807621135342970 ) ) ;
#5866 = CARTESIAN_POINT ( 'NONE',  ( -82.39999999999999147, -34.30312499938548143, 96.81714838363319586 ) ) ;
#5867 = AXIS2_PLACEMENT_3D ( 'NONE', #17608, #12825, #18790 ) ;
#5868 = ORIENTED_EDGE ( 'NONE', *, *, #7452, .F. ) ;
#5869 = VERTEX_POINT ( 'NONE', #16699 ) ;
#5870 = CARTESIAN_POINT ( 'NONE',  ( -82.85293433259495544, -32.00000000000000000, 97.19890519204300006 ) ) ;
#5871 = CARTESIAN_POINT ( 'NONE',  ( 113.0000000000000000, 15.19999999999996732, -143.3166247903554336 ) ) ;
#5872 = ORIENTED_EDGE ( 'NONE', *, *, #7090, .F. ) ;
#5873 = CARTESIAN_POINT ( 'NONE',  ( -80.07894310789832559, -35.00000000000000711, 101.4973817956044684 ) ) ;
#5874 = DIRECTION ( 'NONE',  ( 0.000000000000000000, 0.000000000000000000, 1.000000000000000000 ) ) ;
#5875 = CARTESIAN_POINT ( 'NONE',  ( -6.259644161404859044E-16, -4.618802153517026277, -3.504271511727133248 ) ) ;
#5876 = AXIS2_PLACEMENT_3D ( 'NONE', #7777, #3275, #6320 ) ;
#5877 = VECTOR ( 'NONE', #8821, 1000.000000000000000 ) ;
#5878 = CARTESIAN_POINT ( 'NONE',  ( -85.15643035625001289, -34.30312499938548854, 99.99999999999998579 ) ) ;
#5879 = CARTESIAN_POINT ( 'NONE',  ( -85.40000000000000568, -31.38749999999999574, 98.26794919243111792 ) ) ;
#5880 = CARTESIAN_POINT ( 'NONE',  ( -85.40000000000000568, -31.33124999877096428, 98.26794919243111792 ) ) ;
#5881 = CARTESIAN_POINT ( 'NONE',  ( 235.3193635794330589, -31.99999999999998579, -51.26521311181414831 ) ) ;
#5882 = AXIS2_PLACEMENT_3D ( 'NONE', #17351, #18528, #8547 ) ;
#5883 = CARTESIAN_POINT ( 'NONE',  ( -84.69814120060431151, -35.16451018433117781, 98.07164655156650213 ) ) ;
#5884 = CARTESIAN_POINT ( 'NONE',  ( 244.7999999999999545, -34.51168759575592304, 150.0000000000000000 ) ) ;
#5885 = CARTESIAN_POINT ( 'NONE',  ( 232.5999999999999375, -30.92812499938547433, 103.1828516163667899 ) ) ;
#5886 = ORIENTED_EDGE ( 'NONE', *, *, #8993, .F. ) ;
#5887 = CARTESIAN_POINT ( 'NONE',  ( -82.39999999999999147, -35.09062499938548285, -96.81714838363319586 ) ) ;
#5888 = CARTESIAN_POINT ( 'NONE',  ( 4.140404888673277384, 2.228338276487440428, -3.686887068327033390 ) ) ;
#5889 = VECTOR ( 'NONE', #3397, 1000.000000000000000 ) ;
#5890 = CARTESIAN_POINT ( 'NONE',  ( 3.679171394226031122, 2.494631558665830973, -0.3503314178412474389 ) ) ;
#5891 = CARTESIAN_POINT ( 'NONE',  ( -82.40000000000001990, -32.75624999877096855, 97.00000000000000000 ) ) ;
#5892 = CARTESIAN_POINT ( 'NONE',  ( -82.39999999999999147, -32.05312499938548854, 96.81714838363319586 ) ) ;
#5893 = CARTESIAN_POINT ( 'NONE',  ( 105.1999999999999744, -31.99999999999999289, -100.0000000000000000 ) ) ;
#5894 = CARTESIAN_POINT ( 'NONE',  ( 229.8435696437499871, -32.35312499938547859, -48.40857419181671162 ) ) ;
#5895 = ADVANCED_FACE ( 'NONE', ( #3698 ), #6737, .F. ) ;
#5896 = EDGE_CURVE ( 'NONE', #10687, #13854, #4988, .T. ) ;
#5897 = VERTEX_POINT ( 'NONE', #16987 ) ;
#5898 = ORIENTED_EDGE ( 'NONE', *, *, #12830, .T. ) ;
#5899 = DIRECTION ( 'NONE',  ( 1.000000000000000000, -1.387778780781445676E-15, -2.407412430484046130E-31 ) ) ;
#5900 = CARTESIAN_POINT ( 'NONE',  ( -83.90000000000000568, -31.42500000000000071, 97.40192378864668399 ) ) ;
#5901 = CARTESIAN_POINT ( 'NONE',  ( -79.39999999999999147, -31.55624999877096926, 101.7320508075688537 ) ) ;
#5902 = CARTESIAN_POINT ( 'NONE',  ( 82.39999999999999147, -33.03750000000000142, 96.53589838486223584 ) ) ;
#5903 = LINE ( 'NONE', #5994, #10857 ) ;
#5904 = CARTESIAN_POINT ( 'NONE',  ( 231.2217848218749339, -32.91562499938547148, 97.61286128772489690 ) ) ;
#5905 = CARTESIAN_POINT ( 'NONE',  ( 229.8435696437499587, -34.67812499938547433, -51.59142580818350154 ) ) ;
#5906 = CARTESIAN_POINT ( 'NONE',  ( 82.39999999999999147, -34.97812499938547859, 96.81714838363319586 ) ) ;
#5907 = EDGE_CURVE ( 'NONE', #422, #8584, #11400, .T. ) ;
#5908 = CARTESIAN_POINT ( 'NONE',  ( 83.77821517812500929, -30.21562499938548285, -97.61286128772489690 ) ) ;
#5909 = CARTESIAN_POINT ( 'NONE',  ( 231.2217848218749339, -35.01562499938548001, -47.61286128772501769 ) ) ;
#5910 = EDGE_CURVE ( 'NONE', #1272, #16645, #5567, .T. ) ;
#5911 = CARTESIAN_POINT ( 'NONE',  ( 85.39999999999999147, -34.97364041986484295, -98.90809577818235709 ) ) ;
#5912 = CARTESIAN_POINT ( 'NONE',  ( 79.64356964375001269, -32.57812499938548001, -98.40857419181659793 ) ) ;
#5913 = VERTEX_POINT ( 'NONE', #9855 ) ;
#5914 = CARTESIAN_POINT ( 'NONE',  ( 249.9999999999999716, -5.000000000000004441, -100.0000000000000000 ) ) ;
#5915 = CARTESIAN_POINT ( 'NONE',  ( 81.59615242270662350, -33.91740381056766296, -103.0000000000000000 ) ) ;
#5916 = CARTESIAN_POINT ( 'NONE',  ( -85.40000000000000568, -34.95000000000000284, 99.99999999999998579 ) ) ;
#5917 = CARTESIAN_POINT ( 'NONE',  ( -85.40000000000000568, -31.35000000000000142, 99.99999999999998579 ) ) ;
#5918 = EDGE_LOOP ( 'NONE', ( #1075, #10488, #9411, #4582 ) ) ;
#5919 = CARTESIAN_POINT ( 'NONE',  ( -4.024497503033714452, -2.323544716729502468, -3.572167766733752803 ) ) ;
#5920 = CARTESIAN_POINT ( 'NONE',  ( 233.9782151781249411, -34.34062499938547575, 97.61286128772489690 ) ) ;
#5921 = CARTESIAN_POINT ( 'NONE',  ( 0.000000000000000000, 0.000000000000000000, -5.000000000000000888 ) ) ;
#5922 =( BOUNDED_SURFACE ( )  B_SPLINE_SURFACE ( 1, 2, ( 
 ( #2315, #10920, #2134, #13944, #18645, #12776, #14230, #772, #4979, #5071, #15417, #2028, #3881, #584, #12482, #11310, #9844, #679, #18745, #2413, #14136, #9550, #8281, #5364, #17277, #14328, #12672, #3590, #967, #18450, #16978, #15616, #8091, #14044, #6630, #12579, #5268, #5162, #11108, #17076, #9656, #11213, #4174, #15998, #7292, #18841, #7198, #7107, #2601, #2700, #6922, #17368, #14515, #8562, #3980, #15902, #18935, #13063, #1246, #16197, #2804, #13147, #2898, #19028, #12965, #9945, #8756, #14615, #7010, #17467, #8658, #14708, #13247, #4367, #5650, #1346, #2508, #5556, #19219, #11595, #1149, #8465, #19122, #16094, #17760, #17563, #5464, #10135, #12870, #5740, #5836, #11689, #17658, #11505, #8852, #4078, #1056, #11407, #14808, #4270, #10327, #10231, #16286, #10039, #11788, #14421, #15194, #15103, #4761, #1434, #15010, #10704, #369, #5934, #3274, #7488, #7584, #12173, #13729, #13443, #16481, #2989, #3085, #16669, #17695, #10513, #8944, #7673, #1812, #9232, #9139, #7389, #77, #11881, #13350 ),
 ( #12273, #9046, #7776, #10798, #10611, #17945, #6319, #18236, #18141, #4853, #16578, #11977, #16761, #3377, #6030, #4661, #1628, #4557, #17849, #1718, #13534, #9328, #173, #6124, #4462, #10416, #12075, #14911, #13628, #16379, #1540, #272, #18051, #3178, #6225, #7869, #6807, #12367, #18334, #14207, #12753, #3568, #17152, #5343, #5140, #12459, #18622, #3760, #6704, #844, #11085, #6514, #5240, #18722, #557, #18523, #5046, #18426, #4953, #3667, #10988, #2293, #16956, #14021, #9527, #17055, #11283, #12648, #656, #17251, #3857, #12552, #15493, #15689, #13821, #15594, #2105, #8066, #9631, #15293, #6411, #6604, #2202, #10895, #16863, #7964, #8163, #14112, #11189, #9725, #749, #1907, #8257, #2005, #3469, #463, #9426, #15395, #13919, #5629, #11670, #10209, #7271, #8541, #17635, #18819, #15883, #4249, #14492, #18912, #6899, #17538, #19009, #1323, #17446, #8353, #10016, #9820, #11575, #5721, #8635, #2676, #8445, #11764, #2487, #3956, #15782, #5815, #1123, #13226, #15974, #19199, #12941, #4153, #10114 ) ),
 .UNSPECIFIED., .F., .F., .F. ) 
 B_SPLINE_SURFACE_WITH_KNOTS ( ( 2, 2 ),
 ( 3, 2, 2, 2, 2, 2, 2, 2, 2, 2, 2, 2, 2, 2, 2, 2, 2, 2, 2, 2, 2, 2, 2, 2, 2, 2, 2, 2, 2, 2, 2, 2, 2, 2, 2, 2, 2, 2, 2, 2, 2, 2, 2, 2, 2, 2, 2, 2, 2, 2, 2, 2, 2, 2, 2, 2, 2, 2, 2, 2, 2, 2, 2, 2, 2, 2, 2, 3 ),
 ( 0.000000000000000000, 1.000000000000000000 ),
 ( 0.000000000000000000, 0.01388888888888888812, 0.02777777777777777624, 0.04166666666666666435, 0.05555555555555555247, 0.06944444444444444753, 0.08333333333333332871, 0.09722222222222222376, 0.1111111111111111049, 0.1250000000000000000, 0.1388888888888888951, 0.1527777777777777901, 0.1666666666666666574, 0.1805555555555555525, 0.1944444444444444475, 0.2083333333333333426, 0.2222222222222222099, 0.2361111111111111049, 0.2500000000000000000, 0.2638888888888888951, 0.2777777777777777901, 0.2916666666666666852, 0.3055555555555555802, 0.3194444444444444198, 0.3333333333333333148, 0.3472222222222222099, 0.3611111111111111049, 0.3750000000000000000, 0.3888888888888888951, 0.4027777777777777901, 0.4166666666666666852, 0.4305555555555555802, 0.4444444444444444198, 0.4583333333333333148, 0.4722222222222222099, 0.4861111111111111049, 0.5000000000000000000, 0.5138888888888888395, 0.5277777777777777901, 0.5416666666666666297, 0.5555555555555555802, 0.5694444444444444198, 0.5833333333333333703, 0.5972222222222222099, 0.6111111111111111605, 0.6250000000000000000, 0.6388888888888888395, 0.6527777777777777901, 0.6666666666666666297, 0.6805555555555555802, 0.6944444444444444198, 0.7083333333333333703, 0.7222222222222222099, 0.7361111111111111605, 0.7500000000000000000, 0.7638888888888888395, 0.7777777777777777901, 0.7916666666666666297, 0.8055555555555555802, 0.8194444444444444198, 0.8333333333333333703, 0.8472222222222222099, 0.8611111111111111605, 0.8750000000000000000, 0.8888888888888888395, 0.9027777777777777901, 0.9166666666666666297, 0.9258785144422092550 ),
 .UNSPECIFIED. ) 
 GEOMETRIC_REPRESENTATION_ITEM ( )  RATIONAL_B_SPLINE_SURFACE ( (
 ( 1.000000000000000000, 0.8660254037844387076, 1.000000000000000000, 0.8660254037844387076, 1.000000000000000000, 0.8660254037844387076, 1.000000000000000000, 0.8660254037844387076, 1.000000000000000000, 0.8660254037844387076, 1.000000000000000000, 0.8660254037844387076, 1.000000000000000000, 0.8660254037844387076, 1.000000000000000000, 0.8660254037844387076, 1.000000000000000000, 0.8660254037844387076, 1.000000000000000000, 0.8660254037844387076, 1.000000000000000000, 0.8660254037844387076, 1.000000000000000000, 0.8660254037844387076, 1.000000000000000000, 0.8660254037844387076, 1.000000000000000000, 0.8660254037844387076, 1.000000000000000000, 0.8660254037844387076, 1.000000000000000000, 0.8660254037844387076, 1.000000000000000000, 0.8660254037844387076, 1.000000000000000000, 0.8660254037844387076, 1.000000000000000000, 0.8660254037844387076, 1.000000000000000000, 0.8660254037844387076, 1.000000000000000000, 0.8660254037844387076, 1.000000000000000000, 0.8660254037844387076, 1.000000000000000000, 0.8660254037844387076, 1.000000000000000000, 0.8660254037844387076, 1.000000000000000000, 0.8660254037844387076, 1.000000000000000000, 0.8660254037844387076, 1.000000000000000000, 0.8660254037844387076, 1.000000000000000000, 0.8660254037844387076, 1.000000000000000000, 0.8660254037844387076, 1.000000000000000000, 0.8660254037844387076, 1.000000000000000000, 0.8660254037844387076, 1.000000000000000000, 0.8660254037844387076, 1.000000000000000000, 0.8660254037844387076, 1.000000000000000000, 0.8660254037844387076, 1.000000000000000000, 0.8660254037844387076, 1.000000000000000000, 0.8660254037844387076, 1.000000000000000000, 0.8660254037844387076, 1.000000000000000000, 0.8660254037844387076, 1.000000000000000000, 0.8660254037844387076, 1.000000000000000000, 0.8660254037844387076, 1.000000000000000000, 0.8660254037844387076, 1.000000000000000000, 0.8660254037844387076, 1.000000000000000000, 0.8660254037844387076, 1.000000000000000000, 0.8660254037844387076, 1.000000000000000000, 0.8660254037844387076, 1.000000000000000000, 0.8660254037844387076, 1.000000000000000000, 0.8660254037844387076, 1.000000000000000000, 0.8660254037844387076, 1.000000000000000000, 0.8660254037844387076, 1.000000000000000000, 0.8660254037844387076, 1.000000000000000000, 0.8660254037844387076, 1.000000000000000000, 0.8660254037844387076, 1.000000000000000000, 0.8660254037844387076, 1.000000000000000000, 0.8660254037844387076, 1.000000000000000000, 0.8660254037844387076, 1.000000000000000000, 0.8660254037844387076, 1.000000000000000000, 0.8660254037844387076, 1.000000000000000000, 0.8660254037844387076, 1.000000000000000000, 0.8660254037844387076, 1.000000000000000000, 0.8660254037844387076, 1.000000000000000000, 0.8660254037844387076, 1.000000000000000000, 0.8660254037844387076, 1.000000000000000000, 0.8660254037844387076, 1.000000000000000000, 0.8660254037844387076, 1.000000000000000000, 0.8660254037844387076, 1.000000000000000000, 0.8660254037844387076, 1.000000000000000000, 0.9111409417988175496, 0.9401539645359766606),
 ( 1.000000000000000000, 0.8660254037844387076, 1.000000000000000000, 0.8660254037844387076, 1.000000000000000000, 0.8660254037844387076, 1.000000000000000000, 0.8660254037844387076, 1.000000000000000000, 0.8660254037844387076, 1.000000000000000000, 0.8660254037844387076, 1.000000000000000000, 0.8660254037844387076, 1.000000000000000000, 0.8660254037844387076, 1.000000000000000000, 0.8660254037844387076, 1.000000000000000000, 0.8660254037844387076, 1.000000000000000000, 0.8660254037844387076, 1.000000000000000000, 0.8660254037844387076, 1.000000000000000000, 0.8660254037844387076, 1.000000000000000000, 0.8660254037844387076, 1.000000000000000000, 0.8660254037844387076, 1.000000000000000000, 0.8660254037844387076, 1.000000000000000000, 0.8660254037844387076, 1.000000000000000000, 0.8660254037844387076, 1.000000000000000000, 0.8660254037844387076, 1.000000000000000000, 0.8660254037844387076, 1.000000000000000000, 0.8660254037844387076, 1.000000000000000000, 0.8660254037844387076, 1.000000000000000000, 0.8660254037844387076, 1.000000000000000000, 0.8660254037844387076, 1.000000000000000000, 0.8660254037844387076, 1.000000000000000000, 0.8660254037844387076, 1.000000000000000000, 0.8660254037844387076, 1.000000000000000000, 0.8660254037844387076, 1.000000000000000000, 0.8660254037844387076, 1.000000000000000000, 0.8660254037844387076, 1.000000000000000000, 0.8660254037844387076, 1.000000000000000000, 0.8660254037844387076, 1.000000000000000000, 0.8660254037844387076, 1.000000000000000000, 0.8660254037844387076, 1.000000000000000000, 0.8660254037844387076, 1.000000000000000000, 0.8660254037844387076, 1.000000000000000000, 0.8660254037844387076, 1.000000000000000000, 0.8660254037844387076, 1.000000000000000000, 0.8660254037844387076, 1.000000000000000000, 0.8660254037844387076, 1.000000000000000000, 0.8660254037844387076, 1.000000000000000000, 0.8660254037844387076, 1.000000000000000000, 0.8660254037844387076, 1.000000000000000000, 0.8660254037844387076, 1.000000000000000000, 0.8660254037844387076, 1.000000000000000000, 0.8660254037844387076, 1.000000000000000000, 0.8660254037844387076, 1.000000000000000000, 0.8660254037844387076, 1.000000000000000000, 0.8660254037844387076, 1.000000000000000000, 0.8660254037844387076, 1.000000000000000000, 0.8660254037844387076, 1.000000000000000000, 0.8660254037844387076, 1.000000000000000000, 0.8660254037844387076, 1.000000000000000000, 0.8660254037844387076, 1.000000000000000000, 0.8660254037844387076, 1.000000000000000000, 0.8660254037844387076, 1.000000000000000000, 0.8660254037844387076, 1.000000000000000000, 0.8660254037844387076, 1.000000000000000000, 0.8660254037844387076, 1.000000000000000000, 0.8660254037844387076, 1.000000000000000000, 0.8660254037844387076, 1.000000000000000000, 0.8660254037844387076, 1.000000000000000000, 0.8660254037844387076, 1.000000000000000000, 0.8660254037844387076, 1.000000000000000000, 0.8660254037844387076, 1.000000000000000000, 0.8660254037844387076, 1.000000000000000000, 0.9111409417988175496, 0.9401539645359766606) ) ) 
 REPRESENTATION_ITEM ( '' )  SURFACE ( )  );
#5923 = CARTESIAN_POINT ( 'NONE',  ( -85.40000000000000568, -33.10856250001229739, 101.7320508075688679 ) ) ;
#5924 = PLANE ( 'NONE',  #7657 ) ;
#5925 = CARTESIAN_POINT ( 'NONE',  ( 232.8441546701661480, -32.00000000000000000, -47.13032736203121686 ) ) ;
#5926 = CARTESIAN_POINT ( 'NONE',  ( -82.39999999999999147, -31.15312499938548640, 96.81714838363319586 ) ) ;
#5927 = CARTESIAN_POINT ( 'NONE',  ( 84.28136653320183314, -32.00000000000000711, 102.0145392219077394 ) ) ;
#5928 = CARTESIAN_POINT ( 'NONE',  ( 85.15643035624999868, -32.09062499938548996, 101.5914258081833879 ) ) ;
#5929 = CARTESIAN_POINT ( 'NONE',  ( 82.40000000000000568, -32.08124999877097139, 97.00000000000000000 ) ) ;
#5930 = PLANE ( 'NONE',  #1212 ) ;
#5931 = CARTESIAN_POINT ( 'NONE',  ( -82.39999999999999147, -32.84062499938548996, 103.1828516163667899 ) ) ;
#5932 = CARTESIAN_POINT ( 'NONE',  ( -81.02178482187500208, -31.90312499938548996, -97.61286128772489690 ) ) ;
#5933 = VERTEX_POINT ( 'NONE', #1258 ) ;
#5934 = CARTESIAN_POINT ( 'NONE',  ( 79.39999999999999147, -34.63124999877096855, 101.7320508075688821 ) ) ;
#5935 = CARTESIAN_POINT ( 'NONE',  ( -82.40000000000000568, -30.00000000000000355, 99.99999999999998579 ) ) ;
#5936 = CARTESIAN_POINT ( 'NONE',  ( 233.9782151781249411, -34.90312499938547575, -52.38713871227520968 ) ) ;
#5937 = CARTESIAN_POINT ( 'NONE',  ( -82.39999999999999147, -32.16562499938549280, 96.81714838363319586 ) ) ;
#5938 = FACE_OUTER_BOUND ( 'NONE', #4970, .T. ) ;
#5939 = ORIENTED_EDGE ( 'NONE', *, *, #15263, .T. ) ;
#5940 = CARTESIAN_POINT ( 'NONE',  ( -79.64356964375001269, -33.92812499938548854, -101.5914258081833879 ) ) ;
#5941 = CARTESIAN_POINT ( 'NONE',  ( 2.000000000000005329, -3.464101615137751722, 0.000000000000000000 ) ) ;
#5942 = DIRECTION ( 'NONE',  ( 0.000000000000000000, 0.000000000000000000, 1.000000000000000000 ) ) ;
#5943 = ADVANCED_FACE ( 'NONE', ( #17377 ), #15720, .F. ) ;
#5944 = CARTESIAN_POINT ( 'NONE',  ( -83.77821517812500929, -33.47812499938548569, -102.3871387122750889 ) ) ;
#5945 = CARTESIAN_POINT ( 'NONE',  ( 229.5999999999999375, -33.58124999877096428, -51.73205080756898866 ) ) ;
#5946 = CARTESIAN_POINT ( 'NONE',  ( -79.39999999999999147, -31.51874999877096784, -99.99999999999998579 ) ) ;
#5947 = CARTESIAN_POINT ( 'NONE',  ( 231.2217848218749339, -33.02812499938547575, 97.61286128772489690 ) ) ;
#5948 = CARTESIAN_POINT ( 'NONE',  ( -83.90000000000000568, -31.22268749875867755, 102.5980762113533018 ) ) ;
#5949 = CARTESIAN_POINT ( 'NONE',  ( -85.15643035624999868, -33.81562499938549138, 101.5914258081833879 ) ) ;
#5950 = CARTESIAN_POINT ( 'NONE',  ( -83.77821517812500929, -34.26562499938548711, -102.3871387122750889 ) ) ;
#5951 = CARTESIAN_POINT ( 'NONE',  ( 83.77821517812500929, -32.46562499938548285, 102.3871387122750889 ) ) ;
#5952 =( BOUNDED_CURVE ( )  B_SPLINE_CURVE ( 2, ( #16300, #8674, #4282, #7500, #10526, #3001, #2910, #2815, #186 ),
 .UNSPECIFIED., .F., .F. ) 
 B_SPLINE_CURVE_WITH_KNOTS ( ( 3, 2, 2, 2, 3 ),
 ( 0.8125000000000000000, 0.8194444444444444198, 0.8333333333333333703, 0.8472222222222222099, 0.8541666666666668517 ),
 .UNSPECIFIED. ) 
 CURVE ( )  GEOMETRIC_REPRESENTATION_ITEM ( )  RATIONAL_B_SPLINE_CURVE ( ( 0.9330127018922194093, 0.9330127018922194093, 1.000000000000000000, 0.8660254037844387076, 1.000000000000000000, 0.8660254037844387076, 1.000000000000000000, 0.9330127018922177440, 0.9330127018922194093 ) ) 
 REPRESENTATION_ITEM ( '' )  );
#5953 = CARTESIAN_POINT ( 'NONE',  ( 82.40000000000000568, -30.00000000000000355, 99.99999999999998579 ) ) ;
#5954 = CARTESIAN_POINT ( 'NONE',  ( 79.39999999999999147, -34.66874999877096997, -99.99999999999998579 ) ) ;
#5955 = CARTESIAN_POINT ( 'NONE',  ( 229.5999999999999375, -33.60000000000000142, 99.99999999999998579 ) ) ;
#5956 = EDGE_LOOP ( 'NONE', ( #9662, #13188, #16962, #8487 ) ) ;
#5957 = CARTESIAN_POINT ( 'NONE',  ( 83.77821517812500929, -34.56562499938548427, -102.3871387122750889 ) ) ;
#5958 = CARTESIAN_POINT ( 'NONE',  ( 95.00000000000000000, 10.19999999999994600, -140.0000000000000000 ) ) ;
#5959 = CARTESIAN_POINT ( 'NONE',  ( 229.5999999999999375, -34.89374999877096428, 99.99999999999998579 ) ) ;
#5960 = CARTESIAN_POINT ( 'NONE',  ( 229.5999999999999375, -32.60624999877096997, -48.26794919243123161 ) ) ;
#5962 = ADVANCED_FACE ( 'NONE', ( #18849 ), #7204, .T. ) ;
#5961 = CARTESIAN_POINT ( 'NONE',  ( -85.15643035625001289, -32.42812499938548854, 98.40857419181659793 ) ) ;
#5963 = EDGE_LOOP ( 'NONE', ( #19204, #3666, #18653, #11049, #6520, #5395, #9978, #8117, #17109, #8816, #2180, #2063, #16723, #1722, #11580, #4319, #5273 ) ) ;
#5964 = ORIENTED_EDGE ( 'NONE', *, *, #14175, .F. ) ;
#5965 = DIRECTION ( 'NONE',  ( 0.000000000000000000, 0.000000000000000000, 1.000000000000000000 ) ) ;
#5966 = CARTESIAN_POINT ( 'NONE',  ( -4.211399284164270895, 2.459729995988205964, -3.751162237960538715 ) ) ;
#5967 = CYLINDRICAL_SURFACE ( 'NONE', #15983, 3.000000000000002665 ) ;
#5968 = ORIENTED_EDGE ( 'NONE', *, *, #6579, .F. ) ;
#5969 = CARTESIAN_POINT ( 'NONE',  ( 82.40000000000000568, -32.30624999877097281, -97.00000000000000000 ) ) ;
#5970 = CARTESIAN_POINT ( 'NONE',  ( -94.79999999999999716, -29.80000000000000426, 150.0000000000000000 ) ) ;
#5971 = CARTESIAN_POINT ( 'NONE',  ( -79.64356964374999848, -33.62812499938548427, 99.99999999999998579 ) ) ;
#5972 = CARTESIAN_POINT ( 'NONE',  ( -79.39999999999999147, -33.86250000000000426, 101.7320508075688537 ) ) ;
#5973 = CARTESIAN_POINT ( 'NONE',  ( -79.39999999999999147, -31.10624999877097352, 101.7320508075688537 ) ) ;
#5974 = FACE_OUTER_BOUND ( 'NONE', #12503, .T. ) ;
#5975 =( NAMED_UNIT ( * ) PLANE_ANGLE_UNIT ( ) SI_UNIT ( $, .RADIAN. ) );
#5976 = CARTESIAN_POINT ( 'NONE',  ( -81.59615242270665192, -33.28259618943233278, 97.00000000000000000 ) ) ;
#5977 = CARTESIAN_POINT ( 'NONE',  ( 94.79999999999991189, -3.000000000000000000, 150.0000000000000000 ) ) ;
#5978 = CARTESIAN_POINT ( 'NONE',  ( -85.40000000000000568, -34.50000000000000000, -99.99999999999998579 ) ) ;
#5979 = ORIENTED_EDGE ( 'NONE', *, *, #16290, .F. ) ;
#5980 = CARTESIAN_POINT ( 'NONE',  ( -85.15643035624999868, -34.15312499938548285, -98.40857419181659793 ) ) ;
#5981 = CARTESIAN_POINT ( 'NONE',  ( -83.90000000000000568, -33.52499999999999858, 102.5980762113533018 ) ) ;
#5982 = DIRECTION ( 'NONE',  ( 0.000000000000000000, -1.000000000000000000, 0.000000000000000000 ) ) ;
#5983 = DIRECTION ( 'NONE',  ( -0.000000000000000000, -1.000000000000000000, -0.000000000000000000 ) ) ;
#5984 = CARTESIAN_POINT ( 'NONE',  ( -79.64356964375001269, -31.67812499938548143, 98.40857419181659793 ) ) ;
#5985 = CYLINDRICAL_SURFACE ( 'NONE', #6628, 2.500000000000000444 ) ;
#5986 = CARTESIAN_POINT ( 'NONE',  ( 235.3564303562499447, -32.57812499938547290, -51.59142580818350865 ) ) ;
#5987 =( BOUNDED_CURVE ( )  B_SPLINE_CURVE ( 2, ( #11639, #6870, #17600, #4213, #10172, #11730, #16135, #2745, #8706 ),
 .UNSPECIFIED., .F., .F. ) 
 B_SPLINE_CURVE_WITH_KNOTS ( ( 3, 2, 2, 2, 3 ),
 ( 0.3541666666666666852, 0.3611111111111111049, 0.3750000000000000000, 0.3888888888888888951, 0.3958333333333333703 ),
 .UNSPECIFIED. ) 
 CURVE ( )  GEOMETRIC_REPRESENTATION_ITEM ( )  RATIONAL_B_SPLINE_CURVE ( ( 0.9330127018922194093, 0.9330127018922196314, 1.000000000000000000, 0.8660254037844387076, 1.000000000000000000, 0.8660254037844387076, 1.000000000000000000, 0.9330127018922190762, 0.9330127018922194093 ) ) 
 REPRESENTATION_ITEM ( '' )  );
#5988 = ORIENTED_EDGE ( 'NONE', *, *, #19190, .T. ) ;
#5989 = ORIENTED_EDGE ( 'NONE', *, *, #892, .F. ) ;
#5990 = CARTESIAN_POINT ( 'NONE',  ( 1.567478505476134606E-15, 4.618802153517012066, -3.433295621305382905 ) ) ;
#5991 = CARTESIAN_POINT ( 'NONE',  ( -80.90000000000000568, -30.75000000000000355, 102.5980762113533018 ) ) ;
#5992 = CARTESIAN_POINT ( 'NONE',  ( -82.39999999999999147, -31.18124999877096926, 103.4641016151377499 ) ) ;
#5993 = CARTESIAN_POINT ( 'NONE',  ( 79.39999999999999147, -32.51250000000000284, 98.26794919243113213 ) ) ;
#5994 = CARTESIAN_POINT ( 'NONE',  ( 69.99999999999998579, -34.99999999999999289, 150.0000000000000000 ) ) ;
#5995 = CARTESIAN_POINT ( 'NONE',  ( 233.9782151781249411, -34.04062499938547859, 102.3871387122750889 ) ) ;
#5996 = CARTESIAN_POINT ( 'NONE',  ( 229.8435696437499303, -34.19062499938547717, -50.00000000000011369 ) ) ;
#5997 = CARTESIAN_POINT ( 'NONE',  ( 83.20384757729335945, -33.00134618820329990, -102.9999999999999858 ) ) ;
#5998 = VECTOR ( 'NONE', #16851, 1000.000000000000000 ) ;
#5999 = PRESENTATION_LAYER_ASSIGNMENT (  '', '', ( #3490 ) ) ;
#6000 = CARTESIAN_POINT ( 'NONE',  ( 85.15643035624999868, -31.97812499938548925, -98.40857419181659793 ) ) ;
#6001 = ORIENTED_EDGE ( 'NONE', *, *, #2788, .F. ) ;
#6002 = CARTESIAN_POINT ( 'NONE',  ( 231.2217848218749339, -34.56562499938547717, -47.61286128772501769 ) ) ;
#6003 = CARTESIAN_POINT ( 'NONE',  ( 83.77821517812500929, -33.81562499938548427, -97.61286128772489690 ) ) ;
#6004 = CARTESIAN_POINT ( 'NONE',  ( 109.9999999999999432, -29.80000000000002558, -150.0000000000000000 ) ) ;
#6005 = CARTESIAN_POINT ( 'NONE',  ( -85.40000000000000568, -34.85624999877096997, 101.7320508075688821 ) ) ;
#6006 = CARTESIAN_POINT ( 'NONE',  ( 229.8435696437499871, -32.01562499938548001, -48.40857419181671162 ) ) ;
#6007 = CARTESIAN_POINT ( 'NONE',  ( -82.39999999999999147, -31.46250000000000568, 96.53589838486223584 ) ) ;
#6008 = ORIENTED_EDGE ( 'NONE', *, *, #12151, .T. ) ;
#6009 = CARTESIAN_POINT ( 'NONE',  ( -4.000000000000000000, -2.309401076758512694, -3.433295621305382461 ) ) ;
#6010 = CIRCLE ( 'NONE', #3507, 2.649999999999982148 ) ;
#6011=STYLED_ITEM('',(#19371),#1125);
#6012 = ADVANCED_FACE ( 'NONE', ( #11416 ), #2610, .F. ) ;
#6014 = EDGE_CURVE ( 'NONE', #7316, #2256, #14336, .T. ) ;
#6013 = B_SPLINE_CURVE_WITH_KNOTS ( 'NONE', 3,
 ( #10868, #13888, #13795, #6384, #6097, #9109, #10485, #16642, #3445, #15073, #3244, #1693, #16550, #12045, #12147, #13600, #16839, #6292 ),
 .UNSPECIFIED., .F., .F.,
 ( 4, 2, 2, 2, 2, 2, 2, 2, 4 ),
 ( 0.000000000000000000, 0.0007089252359966436746, 0.001417850471993287349, 0.002126775707989931024, 0.002835700943986574699, 0.003544626179983218373, 0.004253551415979862048, 0.004962476651976506156, 0.005671401887973149397 ),
 .UNSPECIFIED. ) ;
#6015 = CARTESIAN_POINT ( 'NONE',  ( -79.39999999999999147, -31.10624999877097352, 101.7320508075688537 ) ) ;
#6016 = DIRECTION ( 'NONE',  ( -1.000000000000000000, 0.000000000000000000, 0.000000000000000000 ) ) ;
#6017 = CARTESIAN_POINT ( 'NONE',  ( -82.39999999999999147, -33.25856250001228887, 96.53589838486223584 ) ) ;
#6018 = CARTESIAN_POINT ( 'NONE',  ( 0.000000000000000000, -3.031088913245533867, -1.750000000000002220 ) ) ;
#6019 = LINE ( 'NONE', #7573, #1801 ) ;
#6020 = CARTESIAN_POINT ( 'NONE',  ( -83.77821517812500929, -31.11562499938548498, 97.61286128772489690 ) ) ;
#6021 = CARTESIAN_POINT ( 'NONE',  ( -82.39999999999999147, -32.81250000000000000, 97.00000000000000000 ) ) ;
#6022 = CARTESIAN_POINT ( 'NONE',  ( 83.77821517812500929, -32.87812499938548427, 97.61286128772489690 ) ) ;
#6023 = EDGE_CURVE ( 'NONE', #12074, #18433, #5275, .T. ) ;
#6024 = FACE_BOUND ( 'NONE', #16353, .T. ) ;
#6025 = CARTESIAN_POINT ( 'NONE',  ( -82.39999999999999147, -32.36250000000000426, -102.9999999999999858 ) ) ;
#6026 = CARTESIAN_POINT ( 'NONE',  ( -79.64356964374998427, -32.69062499938548427, 98.40857419181659793 ) ) ;
#6027 = DIRECTION ( 'NONE',  ( 1.000000000000000000, 0.000000000000000000, 0.000000000000000000 ) ) ;
#6028 = VECTOR ( 'NONE', #5768, 1000.000000000000000 ) ;
#6029 = ORIENTED_EDGE ( 'NONE', *, *, #5324, .F. ) ;
#6030 = CARTESIAN_POINT ( 'NONE',  ( 83.77821517812500929, -30.77812499938548640, 102.3871387122750889 ) ) ;
#6031 = LINE ( 'NONE', #174, #13336 ) ;
#6032 = CARTESIAN_POINT ( 'NONE',  ( -94.79999999999999716, 0.000000000000000000, 150.0000000000000000 ) ) ;
#6033 = CARTESIAN_POINT ( 'NONE',  ( 4.165266963751924401, -2.049631966911926284, -3.550066703508774069 ) ) ;
#6034 = CARTESIAN_POINT ( 'NONE',  ( -81.02178482187500208, -32.35312499938548569, 102.3871387122750889 ) ) ;
#6035 =( BOUNDED_SURFACE ( )  B_SPLINE_SURFACE ( 1, 2, ( 
 ( #11531, #2446, #14165, #11435, #8305, #4104, #15642, #14446, #17396, #18767, #13086, #7036, #15834, #8588, #12991, #3906, #18963, #4011, #14541, #798, #9974, #19055, #17494, #15928, #2530, #17201, #1177, #10065, #3715, #2626, #5677, #9680, #8491, #8217, #12701, #18675, #9776, #5292, #14353, #11238, #8401, #2344, #14258, #9872, #896, #989, #6855, #12801, #5389, #11335, #17300, #17786, #11, #17976, #3017, #10546, #16122, #4489, #14738, #5960, #16508, #17586, #11908, #8692, #5764, #3111, #15034, #4198, #13469, #1657, #1462, #8784, #16407, #6059, #14941, #9070, #7416, #2830, #1566, #7609, #10159, #14642, #12005, #16315, #1276, #17881, #1373, #4586, #2730, #8975, #13377, #13273, #13561, #7512, #10350, #202, #108, #4393, #11621, #10443, #7223, #13178, #19151, #11716, #17684, #4297, #10261, #16224, #7320, #19248, #5865, #11817, #2924, #8876, #14836, #8094, #10636, #16602, #12197, #2137, #3405, #15519, #16795, #3207, #302, #18264, #9166, #9359, #15130, #15420, #1843, #9454, #1746, #12298, #13846 ),
 ( #394, #14047, #13756, #15319, #6153, #18167, #4789, #13947, #12103, #5075, #7704, #13662, #7801, #6252, #15228, #16892, #16694, #10731, #7896, #2031, #3303, #6440, #12484, #18453, #6346, #7991, #1935, #10923, #18077, #4685, #3495, #4982, #9261, #4880, #10823, #487, #12391, #18360, #588, #6538, #11015, #16981, #3593, #9553, #17370, #11111, #6728, #10042, #5466, #2510, #14140, #775, #2416, #11508, #11216, #8467, #17079, #682, #5558, #12967, #3982, #9948, #18844, #8380, #3884, #9848, #18648, #14232, #5271, #1058, #15811, #870, #4080, #11410, #6835, #12779, #15905, #17181, #18748, #14424, #5165, #9659, #5366, #7014, #6924, #8190, #6633, #18938, #12872, #3785, #12675, #14331, #969, #12582, #17469, #16000, #2319, #9751, #2604, #15715, #8565, #2224, #18548, #3693, #15619, #8283, #11314, #17279, #7200, #13352, #16381, #13445, #2806, #11691, #2703, #19030, #1249, #10516, #5652, #14913, #2900, #10137, #14810, #13617, #5936, #17851, #11979, #1436, #7109, #17762, #16097, #4369, #8661, #2991, #8759 ) ),
 .UNSPECIFIED., .F., .F., .F. ) 
 B_SPLINE_SURFACE_WITH_KNOTS ( ( 2, 2 ),
 ( 3, 2, 2, 2, 2, 2, 2, 2, 2, 2, 2, 2, 2, 2, 2, 2, 2, 2, 2, 2, 2, 2, 2, 2, 2, 2, 2, 2, 2, 2, 2, 2, 2, 2, 2, 2, 2, 2, 2, 2, 2, 2, 2, 2, 2, 2, 2, 2, 2, 2, 2, 2, 2, 2, 2, 2, 2, 2, 2, 2, 2, 2, 2, 2, 2, 2, 2, 3 ),
 ( 0.000000000000000000, 1.000000000000000000 ),
 ( 0.000000000000000000, 0.01388888888888888812, 0.02777777777777777624, 0.04166666666666666435, 0.05555555555555555247, 0.06944444444444444753, 0.08333333333333332871, 0.09722222222222222376, 0.1111111111111111049, 0.1250000000000000000, 0.1388888888888888951, 0.1527777777777777901, 0.1666666666666666574, 0.1805555555555555525, 0.1944444444444444475, 0.2083333333333333426, 0.2222222222222222099, 0.2361111111111111049, 0.2500000000000000000, 0.2638888888888888951, 0.2777777777777777901, 0.2916666666666666852, 0.3055555555555555802, 0.3194444444444444198, 0.3333333333333333148, 0.3472222222222222099, 0.3611111111111111049, 0.3750000000000000000, 0.3888888888888888951, 0.4027777777777777901, 0.4166666666666666852, 0.4305555555555555802, 0.4444444444444444198, 0.4583333333333333148, 0.4722222222222222099, 0.4861111111111111049, 0.5000000000000000000, 0.5138888888888888395, 0.5277777777777777901, 0.5416666666666666297, 0.5555555555555555802, 0.5694444444444444198, 0.5833333333333333703, 0.5972222222222222099, 0.6111111111111111605, 0.6250000000000000000, 0.6388888888888888395, 0.6527777777777777901, 0.6666666666666666297, 0.6805555555555555802, 0.6944444444444444198, 0.7083333333333333703, 0.7222222222222222099, 0.7361111111111111605, 0.7500000000000000000, 0.7638888888888888395, 0.7777777777777777901, 0.7916666666666666297, 0.8055555555555555802, 0.8194444444444444198, 0.8333333333333333703, 0.8472222222222222099, 0.8611111111111111605, 0.8750000000000000000, 0.8888888888888888395, 0.9027777777777777901, 0.9166666666666666297, 0.9258785144422092550 ),
 .UNSPECIFIED. ) 
 GEOMETRIC_REPRESENTATION_ITEM ( )  RATIONAL_B_SPLINE_SURFACE ( (
 ( 1.000000000000000000, 0.8660254037844387076, 1.000000000000000000, 0.8660254037844387076, 1.000000000000000000, 0.8660254037844387076, 1.000000000000000000, 0.8660254037844387076, 1.000000000000000000, 0.8660254037844387076, 1.000000000000000000, 0.8660254037844387076, 1.000000000000000000, 0.8660254037844387076, 1.000000000000000000, 0.8660254037844387076, 1.000000000000000000, 0.8660254037844387076, 1.000000000000000000, 0.8660254037844387076, 1.000000000000000000, 0.8660254037844387076, 1.000000000000000000, 0.8660254037844387076, 1.000000000000000000, 0.8660254037844387076, 1.000000000000000000, 0.8660254037844387076, 1.000000000000000000, 0.8660254037844387076, 1.000000000000000000, 0.8660254037844387076, 1.000000000000000000, 0.8660254037844387076, 1.000000000000000000, 0.8660254037844387076, 1.000000000000000000, 0.8660254037844387076, 1.000000000000000000, 0.8660254037844387076, 1.000000000000000000, 0.8660254037844387076, 1.000000000000000000, 0.8660254037844387076, 1.000000000000000000, 0.8660254037844387076, 1.000000000000000000, 0.8660254037844387076, 1.000000000000000000, 0.8660254037844387076, 1.000000000000000000, 0.8660254037844387076, 1.000000000000000000, 0.8660254037844387076, 1.000000000000000000, 0.8660254037844387076, 1.000000000000000000, 0.8660254037844387076, 1.000000000000000000, 0.8660254037844387076, 1.000000000000000000, 0.8660254037844387076, 1.000000000000000000, 0.8660254037844387076, 1.000000000000000000, 0.8660254037844387076, 1.000000000000000000, 0.8660254037844387076, 1.000000000000000000, 0.8660254037844387076, 1.000000000000000000, 0.8660254037844387076, 1.000000000000000000, 0.8660254037844387076, 1.000000000000000000, 0.8660254037844387076, 1.000000000000000000, 0.8660254037844387076, 1.000000000000000000, 0.8660254037844387076, 1.000000000000000000, 0.8660254037844387076, 1.000000000000000000, 0.8660254037844387076, 1.000000000000000000, 0.8660254037844387076, 1.000000000000000000, 0.8660254037844387076, 1.000000000000000000, 0.8660254037844387076, 1.000000000000000000, 0.8660254037844387076, 1.000000000000000000, 0.8660254037844387076, 1.000000000000000000, 0.8660254037844387076, 1.000000000000000000, 0.8660254037844387076, 1.000000000000000000, 0.8660254037844387076, 1.000000000000000000, 0.8660254037844387076, 1.000000000000000000, 0.8660254037844387076, 1.000000000000000000, 0.8660254037844387076, 1.000000000000000000, 0.8660254037844387076, 1.000000000000000000, 0.8660254037844387076, 1.000000000000000000, 0.8660254037844387076, 1.000000000000000000, 0.8660254037844387076, 1.000000000000000000, 0.8660254037844387076, 1.000000000000000000, 0.8660254037844387076, 1.000000000000000000, 0.8660254037844387076, 1.000000000000000000, 0.8660254037844387076, 1.000000000000000000, 0.8660254037844387076, 1.000000000000000000, 0.8660254037844387076, 1.000000000000000000, 0.8660254037844387076, 1.000000000000000000, 0.8660254037844387076, 1.000000000000000000, 0.8660254037844387076, 1.000000000000000000, 0.9111409417988175496, 0.9401539645359766606),
 ( 1.000000000000000000, 0.8660254037844387076, 1.000000000000000000, 0.8660254037844387076, 1.000000000000000000, 0.8660254037844387076, 1.000000000000000000, 0.8660254037844387076, 1.000000000000000000, 0.8660254037844387076, 1.000000000000000000, 0.8660254037844387076, 1.000000000000000000, 0.8660254037844387076, 1.000000000000000000, 0.8660254037844387076, 1.000000000000000000, 0.8660254037844387076, 1.000000000000000000, 0.8660254037844387076, 1.000000000000000000, 0.8660254037844387076, 1.000000000000000000, 0.8660254037844387076, 1.000000000000000000, 0.8660254037844387076, 1.000000000000000000, 0.8660254037844387076, 1.000000000000000000, 0.8660254037844387076, 1.000000000000000000, 0.8660254037844387076, 1.000000000000000000, 0.8660254037844387076, 1.000000000000000000, 0.8660254037844387076, 1.000000000000000000, 0.8660254037844387076, 1.000000000000000000, 0.8660254037844387076, 1.000000000000000000, 0.8660254037844387076, 1.000000000000000000, 0.8660254037844387076, 1.000000000000000000, 0.8660254037844387076, 1.000000000000000000, 0.8660254037844387076, 1.000000000000000000, 0.8660254037844387076, 1.000000000000000000, 0.8660254037844387076, 1.000000000000000000, 0.8660254037844387076, 1.000000000000000000, 0.8660254037844387076, 1.000000000000000000, 0.8660254037844387076, 1.000000000000000000, 0.8660254037844387076, 1.000000000000000000, 0.8660254037844387076, 1.000000000000000000, 0.8660254037844387076, 1.000000000000000000, 0.8660254037844387076, 1.000000000000000000, 0.8660254037844387076, 1.000000000000000000, 0.8660254037844387076, 1.000000000000000000, 0.8660254037844387076, 1.000000000000000000, 0.8660254037844387076, 1.000000000000000000, 0.8660254037844387076, 1.000000000000000000, 0.8660254037844387076, 1.000000000000000000, 0.8660254037844387076, 1.000000000000000000, 0.8660254037844387076, 1.000000000000000000, 0.8660254037844387076, 1.000000000000000000, 0.8660254037844387076, 1.000000000000000000, 0.8660254037844387076, 1.000000000000000000, 0.8660254037844387076, 1.000000000000000000, 0.8660254037844387076, 1.000000000000000000, 0.8660254037844387076, 1.000000000000000000, 0.8660254037844387076, 1.000000000000000000, 0.8660254037844387076, 1.000000000000000000, 0.8660254037844387076, 1.000000000000000000, 0.8660254037844387076, 1.000000000000000000, 0.8660254037844387076, 1.000000000000000000, 0.8660254037844387076, 1.000000000000000000, 0.8660254037844387076, 1.000000000000000000, 0.8660254037844387076, 1.000000000000000000, 0.8660254037844387076, 1.000000000000000000, 0.8660254037844387076, 1.000000000000000000, 0.8660254037844387076, 1.000000000000000000, 0.8660254037844387076, 1.000000000000000000, 0.8660254037844387076, 1.000000000000000000, 0.8660254037844387076, 1.000000000000000000, 0.8660254037844387076, 1.000000000000000000, 0.8660254037844387076, 1.000000000000000000, 0.8660254037844387076, 1.000000000000000000, 0.8660254037844387076, 1.000000000000000000, 0.8660254037844387076, 1.000000000000000000, 0.9111409417988175496, 0.9401539645359766606) ) ) 
 REPRESENTATION_ITEM ( '' )  SURFACE ( )  );
#6036 = CARTESIAN_POINT ( 'NONE',  ( -84.70388354820684640, -35.00002705695768412, -101.9214814096701076 ) ) ;
#6037 = ORIENTED_EDGE ( 'NONE', *, *, #3662, .F. ) ;
#6038 = CARTESIAN_POINT ( 'NONE',  ( -79.39999999999999147, -31.61250000000000071, -98.26794919243113213 ) ) ;
#6039 = CARTESIAN_POINT ( 'NONE',  ( 4.000000000000000888, 0.8228435280416209752, -3.430609588141487976 ) ) ;
#6040 = EDGE_CURVE ( 'NONE', #17953, #8755, #3888, .T. ) ;
#6041 = DIRECTION ( 'NONE',  ( 0.000000000000000000, 0.000000000000000000, 1.000000000000000000 ) ) ;
#6042 = CARTESIAN_POINT ( 'NONE',  ( -85.15643035624999868, -32.99062499938548854, -101.5914258081833879 ) ) ;
#6043 = EDGE_CURVE ( 'NONE', #4397, #17663, #12973, .T. ) ;
#6044 = CARTESIAN_POINT ( 'NONE',  ( 229.5999999999999375, -33.54374999877096286, -50.00000000000011369 ) ) ;
#6045 = CARTESIAN_POINT ( 'NONE',  ( 229.8435696437499871, -30.66562499938547859, 101.5914258081833879 ) ) ;
#6046 = CARTESIAN_POINT ( 'NONE',  ( -79.39999999999999147, -31.11018749875868394, 101.7320508075688537 ) ) ;
#6047 = CARTESIAN_POINT ( 'NONE',  ( -85.15643035624999868, -33.36562499938548854, 101.5914258081833879 ) ) ;
#6048 = CARTESIAN_POINT ( 'NONE',  ( 235.5999999999999375, -33.76874999877096428, 99.99999999999998579 ) ) ;
#6049 = CARTESIAN_POINT ( 'NONE',  ( 82.39999999999999147, -33.17812499938548854, 96.81714838363319586 ) ) ;
#6050 = DIRECTION ( 'NONE',  ( 1.788378118793198438E-31, 3.597944987211154374E-15, 1.000000000000000000 ) ) ;
#6051 = CARTESIAN_POINT ( 'NONE',  ( 232.5999999999999375, -29.99999999999999645, 103.0000000000000000 ) ) ;
#6052 = CARTESIAN_POINT ( 'NONE',  ( 79.39999999999999147, -33.35624999877097707, -101.7320508075688537 ) ) ;
#6053 = CARTESIAN_POINT ( 'NONE',  ( 234.0999999999999375, -32.39999999999999858, 97.40192378864668399 ) ) ;
#6054 = ORIENTED_EDGE ( 'NONE', *, *, #9967, .T. ) ;
#6055 = CARTESIAN_POINT ( 'NONE',  ( 229.8435696437499303, -34.30312499938548143, -50.00000000000011369 ) ) ;
#6056 = DIRECTION ( 'NONE',  ( 0.000000000000000000, 0.000000000000000000, 1.000000000000000000 ) ) ;
#6057 = EDGE_CURVE ( 'NONE', #6753, #18433, #13151, .T. ) ;
#6058 = CARTESIAN_POINT ( 'NONE',  ( 229.8435696437499871, -30.74062499938547433, 98.40857419181659793 ) ) ;
#6059 = CARTESIAN_POINT ( 'NONE',  ( 229.5999999999999375, -33.13124999877096144, -51.73205080756898866 ) ) ;
#6060 = CARTESIAN_POINT ( 'NONE',  ( -79.64356964374998427, -32.57812499938548711, 98.40857419181659793 ) ) ;
#6061 = VERTEX_POINT ( 'NONE', #8288 ) ;
#6062 = EDGE_LOOP ( 'NONE', ( #17590, #15416, #11161, #11195, #4194, #6758, #3991, #6547, #9540, #11265, #14050, #13820, #11343, #17198, #14327, #490, #13043 ) ) ;
#6063 = LINE ( 'NONE', #18268, #16320 ) ;
#6064 = CARTESIAN_POINT ( 'NONE',  ( -4.000000000000000000, 2.471528634177585282, -3.686887442155186712 ) ) ;
#6065 = CARTESIAN_POINT ( 'NONE',  ( -83.90000000000000568, -33.52499999999999858, -97.40192378864668399 ) ) ;
#6066 = EDGE_LOOP ( 'NONE', ( #17040, #2060, #18457, #8243 ) ) ;
#6067 = CARTESIAN_POINT ( 'NONE',  ( 111.5000000000000142, 12.69999999999998508, 110.0000000000000142 ) ) ;
#6068 = CARTESIAN_POINT ( 'NONE',  ( 234.0999999999999375, -32.39999999999999858, 97.40192378864668399 ) ) ;
#6069 = CARTESIAN_POINT ( 'NONE',  ( -79.64356964375001269, -34.04062499938549280, 98.40857419181659793 ) ) ;
#6070 = CARTESIAN_POINT ( 'NONE',  ( -82.39999999999999147, -33.93750000000000000, 103.4641016151377499 ) ) ;
#6071 =( BOUNDED_CURVE ( )  B_SPLINE_CURVE ( 2, ( #5847, #17861, #11800, #11698, #17769, #4472, #5569, #10243, #14817 ),
 .UNSPECIFIED., .F., .F. ) 
 B_SPLINE_CURVE_WITH_KNOTS ( ( 3, 2, 2, 2, 3 ),
 ( 0.6458333333333332593, 0.6527777777777777901, 0.6666666666666666297, 0.6805555555555555802, 0.6875000000000000000 ),
 .UNSPECIFIED. ) 
 CURVE ( )  GEOMETRIC_REPRESENTATION_ITEM ( )  RATIONAL_B_SPLINE_CURVE ( ( 0.9330127018922192983, 0.9330127018922187432, 1.000000000000000000, 0.8660254037844387076, 1.000000000000000000, 0.8660254037844387076, 1.000000000000000000, 0.9330127018922194093, 0.9330127018922194093 ) ) 
 REPRESENTATION_ITEM ( '' )  );
#6072 = EDGE_CURVE ( 'NONE', #5766, #15452, #14239, .T. ) ;
#6073 = CARTESIAN_POINT ( 'NONE',  ( -82.39999999999999147, -32.53124999877096712, 103.4641016151377499 ) ) ;
#6074 = CYLINDRICAL_SURFACE ( 'NONE', #9761, 2.200000000000007283 ) ;
#6075 = CARTESIAN_POINT ( 'NONE',  ( 81.59615242270662350, -34.63259618943234130, -96.99999999999997158 ) ) ;
#6076 = CARTESIAN_POINT ( 'NONE',  ( -82.39999999999999147, -33.48750000000000426, 103.0000000000000000 ) ) ;
#6077 = CARTESIAN_POINT ( 'NONE',  ( -80.03686793005711309, -35.00000000000002842, -101.6462804658012118 ) ) ;
#6078 = CARTESIAN_POINT ( 'NONE',  ( 229.8435696437499871, -31.07812499938548001, 98.40857419181659793 ) ) ;
#6079 = ORIENTED_EDGE ( 'NONE', *, *, #6040, .F. ) ;
#6080 = APPLICATION_CONTEXT ( 'automotive_design' ) ;
#6081 = CARTESIAN_POINT ( 'NONE',  ( -79.64356964375001269, -33.02812499938548285, -101.5914258081833879 ) ) ;
#6082 = CARTESIAN_POINT ( 'NONE',  ( 235.5999999999999943, -32.43749999999999289, -51.73205080756900287 ) ) ;
#6083 = CARTESIAN_POINT ( 'NONE',  ( 234.0999999999999375, -34.59374999877096002, -52.59807621135342970 ) ) ;
#6084 = CARTESIAN_POINT ( 'NONE',  ( -85.40000000000000568, -32.68124999877097281, 98.26794919243111792 ) ) ;
#6085 = CARTESIAN_POINT ( 'NONE',  ( -81.02178482187500208, -30.29062499938548569, 97.61286128772489690 ) ) ;
#6086 = CARTESIAN_POINT ( 'NONE',  ( 82.40000000000001990, -33.26250000000000284, -97.00000000000000000 ) ) ;
#6087 = CARTESIAN_POINT ( 'NONE',  ( 232.5999999999999375, -31.82812499938547290, -46.81714838363331666 ) ) ;
#6088 = EDGE_LOOP ( 'NONE', ( #19059, #997 ) ) ;
#6089 = ORIENTED_EDGE ( 'NONE', *, *, #16819, .T. ) ;
#6090 = CARTESIAN_POINT ( 'NONE',  ( 0.3126073911696412022, -2.020725942163688504, 3.500000000000000444 ) ) ;
#6091 = CARTESIAN_POINT ( 'NONE',  ( -82.39999999999999147, -31.01249999999999929, 96.53589838486223584 ) ) ;
#6092 = CARTESIAN_POINT ( 'NONE',  ( -85.40000000000000568, -32.64374999877097139, 99.99999999999998579 ) ) ;
#6093 = CARTESIAN_POINT ( 'NONE',  ( 83.90000000000000568, -31.72500000000000142, 97.40192378864668399 ) ) ;
#6094 = CARTESIAN_POINT ( 'NONE',  ( 0.000000000000000000, 3.755786496842896592E-16, -3.499999999999999556 ) ) ;
#6095 = CARTESIAN_POINT ( 'NONE',  ( 235.3564303562499447, -34.82812499938548001, 98.40857419181659793 ) ) ;
#6096 = CARTESIAN_POINT ( 'NONE',  ( 235.3564303562499447, -34.37812499938547717, -51.59142580818350154 ) ) ;
#6097 = CARTESIAN_POINT ( 'NONE',  ( 83.30522522562139898, -31.99999999999999289, -97.33297554272277807 ) ) ;
#6098 = COLOUR_RGB ( '',0.8941176470588234615, 0.8941176470588234615, 0.8941176470588234615 ) ;
#6099 = CARTESIAN_POINT ( 'NONE',  ( 82.39999999999999147, -31.37812499938548427, -103.1828516163667899 ) ) ;
#6100 = ORIENTED_EDGE ( 'NONE', *, *, #528, .F. ) ;
#6101 = CARTESIAN_POINT ( 'NONE',  ( 231.0999999999999375, -33.22499999999999432, -52.59807621135342970 ) ) ;
#6102 = CARTESIAN_POINT ( 'NONE',  ( 82.39999999999999147, -33.17812499938548854, -103.1828516163667899 ) ) ;
#6103 =( BOUNDED_SURFACE ( )  B_SPLINE_SURFACE ( 1, 2, ( 
 ( #1296, #11644, #8804, #19267, #17605, #17800, #2942, #16429, #14761, #12024, #10176, #7438, #14958, #14661, #7243, #7339, #10368, #19171, #8895, #7531, #1197, #5885, #16333, #8609, #128, #6078, #14558, #13395, #28, #4707, #4899, #4609, #16816, #10565, #15249, #15148, #12127, #6365, #16528, #16621, #18098, #3226, #3129, #417, #12218, #9375, #7627, #3425, #9088, #15052, #9185, #1675, #1862, #13581, #221, #6175, #10654, #1766, #7725, #9282, #13682, #325, #6273, #18187, #4809, #10750, #16714, #3321, #12316, #13777, #10844, #7822, #18283, #14065, #6655, #794, #3802, #700, #5287, #9676, #6458, #12411, #5184, #2155, #7820, #18472, #10843, #17099, #12315, #9573, #10941, #18671, #3710, #4898, #2242, #13968, #608, #16908, #13864, #5000, #18282, #11234, #5092, #16815, #3517, #12600, #18380, #17197, #14160, #6363, #8210, #17000, #18570, #6751, #6557, #506, #3612, #15540, #8112, #12502, #9475, #1861, #1955, #15439, #11131, #15637, #11036, #12696, #2050, #416, #15248, #13775, #3424, #9374, #15339, #7915, #8009 ),
 ( #2441, #16116, #14254, #5385, #2725, #12796, #12986, #10061, #16019, #3901, #891, #6851, #15732, #8396, #1074, #14349, #8687, #6941, #5672, #17296, #2621, #4004, #17678, #4097, #11429, #19049, #8583, #14637, #13174, #11527, #17582, #14537, #12891, #15829, #985, #4193, #9770, #14441, #7129, #18862, #18763, #5483, #17392, #1271, #11615, #9969, #11331, #7218, #1172, #9867, #15923, #2526, #7032, #8486, #13081, #18957, #10155, #19144, #5580, #5760, #17490, #11711, #2339, #8301, #6053, #1652, #3202, #13373, #14936, #4681, #6, #7604, #4389, #9161, #14830, #13269, #3011, #13465, #7313, #12000, #16504, #12098, #4484, #6245, #19242, #9065, #18070, #16311, #1457, #8970, #17969, #17781, #3107, #16596, #14733, #7411, #5955, #16219, #7698, #6146, #12192, #10345, #11904, #17875, #15125, #4293, #13655, #10257, #15030, #10437, #2919, #10631, #2824, #16403, #8872, #1561, #297, #13555, #7508, #1740, #1368, #8780, #5860, #103, #11813, #4581, #10538, #197, #14041, #8089, #5067, #11106, #18259, #6723, #14134, #15514, #2131 ) ),
 .UNSPECIFIED., .F., .F., .F. ) 
 B_SPLINE_SURFACE_WITH_KNOTS ( ( 2, 2 ),
 ( 3, 2, 2, 2, 2, 2, 2, 2, 2, 2, 2, 2, 2, 2, 2, 2, 2, 2, 2, 2, 2, 2, 2, 2, 2, 2, 2, 2, 2, 2, 2, 2, 2, 2, 2, 2, 2, 2, 2, 2, 2, 2, 2, 2, 2, 2, 2, 2, 2, 2, 2, 2, 2, 2, 2, 2, 2, 2, 2, 2, 2, 2, 2, 2, 2, 2, 2, 2, 3 ),
 ( 0.000000000000000000, 1.000000000000000000 ),
 ( 0.000000000000000000, 0.01388888888888888812, 0.02777777777777777624, 0.04166666666666666435, 0.05555555555555555247, 0.06944444444444444753, 0.08333333333333332871, 0.09722222222222222376, 0.1111111111111111049, 0.1250000000000000000, 0.1388888888888888951, 0.1527777777777777901, 0.1666666666666666574, 0.1805555555555555525, 0.1944444444444444475, 0.2083333333333333426, 0.2222222222222222099, 0.2361111111111111049, 0.2500000000000000000, 0.2638888888888888951, 0.2777777777777777901, 0.2916666666666666852, 0.3055555555555555802, 0.3194444444444444198, 0.3333333333333333148, 0.3472222222222222099, 0.3611111111111111049, 0.3750000000000000000, 0.3888888888888888951, 0.4027777777777777901, 0.4166666666666666852, 0.4305555555555555802, 0.4444444444444444198, 0.4583333333333333148, 0.4722222222222222099, 0.4861111111111111049, 0.5000000000000000000, 0.5138888888888888395, 0.5277777777777777901, 0.5416666666666666297, 0.5555555555555555802, 0.5694444444444444198, 0.5833333333333333703, 0.5972222222222222099, 0.6111111111111111605, 0.6250000000000000000, 0.6388888888888888395, 0.6527777777777777901, 0.6666666666666666297, 0.6805555555555555802, 0.6944444444444444198, 0.7083333333333333703, 0.7222222222222222099, 0.7361111111111111605, 0.7500000000000000000, 0.7638888888888888395, 0.7777777777777777901, 0.7916666666666666297, 0.8055555555555555802, 0.8194444444444444198, 0.8333333333333333703, 0.8472222222222222099, 0.8611111111111111605, 0.8750000000000000000, 0.8888888888888888395, 0.9027777777777777901, 0.9166666666666666297, 0.9258785066912882389, 0.9351372917582011501 ),
 .UNSPECIFIED. ) 
 GEOMETRIC_REPRESENTATION_ITEM ( )  RATIONAL_B_SPLINE_SURFACE ( (
 ( 1.000000000000000000, 0.8660254037844387076, 1.000000000000000000, 0.8660254037844387076, 1.000000000000000000, 0.8660254037844387076, 1.000000000000000000, 0.8660254037844387076, 1.000000000000000000, 0.8660254037844387076, 1.000000000000000000, 0.8660254037844387076, 1.000000000000000000, 0.8660254037844387076, 1.000000000000000000, 0.8660254037844387076, 1.000000000000000000, 0.8660254037844387076, 1.000000000000000000, 0.8660254037844387076, 1.000000000000000000, 0.8660254037844387076, 1.000000000000000000, 0.8660254037844387076, 1.000000000000000000, 0.8660254037844387076, 1.000000000000000000, 0.8660254037844387076, 1.000000000000000000, 0.8660254037844387076, 1.000000000000000000, 0.8660254037844387076, 1.000000000000000000, 0.8660254037844387076, 1.000000000000000000, 0.8660254037844387076, 1.000000000000000000, 0.8660254037844387076, 1.000000000000000000, 0.8660254037844387076, 1.000000000000000000, 0.8660254037844387076, 1.000000000000000000, 0.8660254037844387076, 1.000000000000000000, 0.8660254037844387076, 1.000000000000000000, 0.8660254037844387076, 1.000000000000000000, 0.8660254037844387076, 1.000000000000000000, 0.8660254037844387076, 1.000000000000000000, 0.8660254037844387076, 1.000000000000000000, 0.8660254037844387076, 1.000000000000000000, 0.8660254037844387076, 1.000000000000000000, 0.8660254037844387076, 1.000000000000000000, 0.8660254037844387076, 1.000000000000000000, 0.8660254037844387076, 1.000000000000000000, 0.8660254037844387076, 1.000000000000000000, 0.8660254037844387076, 1.000000000000000000, 0.8660254037844387076, 1.000000000000000000, 0.8660254037844387076, 1.000000000000000000, 0.8660254037844387076, 1.000000000000000000, 0.8660254037844387076, 1.000000000000000000, 0.8660254037844387076, 1.000000000000000000, 0.8660254037844387076, 1.000000000000000000, 0.8660254037844387076, 1.000000000000000000, 0.8660254037844387076, 1.000000000000000000, 0.8660254037844387076, 1.000000000000000000, 0.8660254037844387076, 1.000000000000000000, 0.8660254037844387076, 1.000000000000000000, 0.8660254037844387076, 1.000000000000000000, 0.8660254037844387076, 1.000000000000000000, 0.8660254037844387076, 1.000000000000000000, 0.8660254037844387076, 1.000000000000000000, 0.8660254037844387076, 1.000000000000000000, 0.8660254037844387076, 1.000000000000000000, 0.8660254037844387076, 1.000000000000000000, 0.8660254037844387076, 1.000000000000000000, 0.8660254037844387076, 1.000000000000000000, 0.8660254037844387076, 1.000000000000000000, 0.8660254037844387076, 1.000000000000000000, 0.8660254037844387076, 1.000000000000000000, 0.8660254037844387076, 1.000000000000000000, 0.8660254037844387076, 1.000000000000000000, 0.8660254037844387076, 1.000000000000000000, 0.8660254037844387076, 1.000000000000000000, 0.8660254037844387076, 1.000000000000000000, 0.8660254037844387076, 1.000000000000000000, 0.8660254037844387076, 1.000000000000000000, 0.8660254037844387076, 1.000000000000000000, 0.8660254037844387076, 1.000000000000000000, 0.9111410165655264848, 0.9401539157124900736, 0.9401539157124900736, 0.9401539157124900736),
 ( 1.000000000000000000, 0.8660254037844387076, 1.000000000000000000, 0.8660254037844387076, 1.000000000000000000, 0.8660254037844387076, 1.000000000000000000, 0.8660254037844387076, 1.000000000000000000, 0.8660254037844387076, 1.000000000000000000, 0.8660254037844387076, 1.000000000000000000, 0.8660254037844387076, 1.000000000000000000, 0.8660254037844387076, 1.000000000000000000, 0.8660254037844387076, 1.000000000000000000, 0.8660254037844387076, 1.000000000000000000, 0.8660254037844387076, 1.000000000000000000, 0.8660254037844387076, 1.000000000000000000, 0.8660254037844387076, 1.000000000000000000, 0.8660254037844387076, 1.000000000000000000, 0.8660254037844387076, 1.000000000000000000, 0.8660254037844387076, 1.000000000000000000, 0.8660254037844387076, 1.000000000000000000, 0.8660254037844387076, 1.000000000000000000, 0.8660254037844387076, 1.000000000000000000, 0.8660254037844387076, 1.000000000000000000, 0.8660254037844387076, 1.000000000000000000, 0.8660254037844387076, 1.000000000000000000, 0.8660254037844387076, 1.000000000000000000, 0.8660254037844387076, 1.000000000000000000, 0.8660254037844387076, 1.000000000000000000, 0.8660254037844387076, 1.000000000000000000, 0.8660254037844387076, 1.000000000000000000, 0.8660254037844387076, 1.000000000000000000, 0.8660254037844387076, 1.000000000000000000, 0.8660254037844387076, 1.000000000000000000, 0.8660254037844387076, 1.000000000000000000, 0.8660254037844387076, 1.000000000000000000, 0.8660254037844387076, 1.000000000000000000, 0.8660254037844387076, 1.000000000000000000, 0.8660254037844387076, 1.000000000000000000, 0.8660254037844387076, 1.000000000000000000, 0.8660254037844387076, 1.000000000000000000, 0.8660254037844387076, 1.000000000000000000, 0.8660254037844387076, 1.000000000000000000, 0.8660254037844387076, 1.000000000000000000, 0.8660254037844387076, 1.000000000000000000, 0.8660254037844387076, 1.000000000000000000, 0.8660254037844387076, 1.000000000000000000, 0.8660254037844387076, 1.000000000000000000, 0.8660254037844387076, 1.000000000000000000, 0.8660254037844387076, 1.000000000000000000, 0.8660254037844387076, 1.000000000000000000, 0.8660254037844387076, 1.000000000000000000, 0.8660254037844387076, 1.000000000000000000, 0.8660254037844387076, 1.000000000000000000, 0.8660254037844387076, 1.000000000000000000, 0.8660254037844387076, 1.000000000000000000, 0.8660254037844387076, 1.000000000000000000, 0.8660254037844387076, 1.000000000000000000, 0.8660254037844387076, 1.000000000000000000, 0.8660254037844387076, 1.000000000000000000, 0.8660254037844387076, 1.000000000000000000, 0.8660254037844387076, 1.000000000000000000, 0.8660254037844387076, 1.000000000000000000, 0.8660254037844387076, 1.000000000000000000, 0.8660254037844387076, 1.000000000000000000, 0.8660254037844387076, 1.000000000000000000, 0.8660254037844387076, 1.000000000000000000, 0.8660254037844387076, 1.000000000000000000, 0.8660254037844387076, 1.000000000000000000, 0.8660254037844387076, 1.000000000000000000, 0.9111410165655264848, 0.9401539157124900736, 0.9401539157124900736, 0.9401539157124900736) ) ) 
 REPRESENTATION_ITEM ( '' )  SURFACE ( )  );
#6104 = FACE_OUTER_BOUND ( 'NONE', #2486, .T. ) ;
#6105 = CARTESIAN_POINT ( 'NONE',  ( -82.40000000000000568, -34.78124999877096712, 102.9999999999999858 ) ) ;
#6106 = CARTESIAN_POINT ( 'NONE',  ( 235.3564303562499447, -30.51562499938548001, -48.40857419181671162 ) ) ;
#6107 = CARTESIAN_POINT ( 'NONE',  ( -79.39999999999999147, -31.12500000000000355, 99.99999999999998579 ) ) ;
#6108 = ORIENTED_EDGE ( 'NONE', *, *, #2563, .F. ) ;
#6109 = CARTESIAN_POINT ( 'NONE',  ( 79.68596062386927770, -32.00000000000000000, 98.72172371342817598 ) ) ;
#6110 = CIRCLE ( 'NONE', #510, 2.500000000000000444 ) ;
#6111 = FACE_OUTER_BOUND ( 'NONE', #11719, .T. ) ;
#6112 = CARTESIAN_POINT ( 'NONE',  ( 79.64356964375001269, -30.77812499938548285, 101.5914258081833879 ) ) ;
#6113 = CARTESIAN_POINT ( 'NONE',  ( -85.40000000000000568, -32.65856250001228744, 101.7320508075688679 ) ) ;
#6114 = CARTESIAN_POINT ( 'NONE',  ( 1.734723475976807094E-15, 4.618802153517012954, -0.4999999999999995559 ) ) ;
#6115 = CARTESIAN_POINT ( 'NONE',  ( 244.7999999999999545, -5.000000000000000888, -103.0000000000000995 ) ) ;
#6116 = CARTESIAN_POINT ( 'NONE',  ( -81.59615242270662350, -32.56740381056766864, 103.0000000000000000 ) ) ;
#6117 = CARTESIAN_POINT ( 'NONE',  ( 83.77821517812500929, -30.51562499938548711, 97.61286128772489690 ) ) ;
#6118 = CARTESIAN_POINT ( 'NONE',  ( -85.40000000000000568, -32.66250000000000142, 101.7320508075688821 ) ) ;
#6119 = LINE ( 'NONE', #11784, #17716 ) ;
#6120 = CARTESIAN_POINT ( 'NONE',  ( 81.02178482187500208, -35.05312499938548854, -102.3871387122750889 ) ) ;
#6121 = CARTESIAN_POINT ( 'NONE',  ( -85.15643035624999868, -31.19062499938548783, -101.5914258081833879 ) ) ;
#6122 = AXIS2_PLACEMENT_3D ( 'NONE', #16856, #5233, #2097 ) ;
#6123 = ORIENTED_EDGE ( 'NONE', *, *, #528, .T. ) ;
#6124 = CARTESIAN_POINT ( 'NONE',  ( 85.15643035624999868, -31.11562499938548854, 98.40857419181659793 ) ) ;
#6125 = DIRECTION ( 'NONE',  ( -1.586032892321652088E-15, -1.000000000000000000, 0.000000000000000000 ) ) ;
#6126 = EDGE_CURVE ( 'NONE', #16779, #15015, #16013, .T. ) ;
#6127 = CARTESIAN_POINT ( 'NONE',  ( -83.90000000000000568, -33.22500000000000142, 97.40192378864668399 ) ) ;
#6128 = CARTESIAN_POINT ( 'NONE',  ( -83.77821517812500929, -31.97812499938548925, 102.3871387122750889 ) ) ;
#6129 = DIRECTION ( 'NONE',  ( -0.000000000000000000, -1.000000000000000000, -0.000000000000000000 ) ) ;
#6130 = VERTEX_POINT ( 'NONE', #18753 ) ;
#6131 = CARTESIAN_POINT ( 'NONE',  ( -82.39999999999999147, -32.13749999999999574, -96.53589838486223584 ) ) ;
#6132 = EDGE_CURVE ( 'NONE', #804, #2622, #11513, .T. ) ;
#6133 = STYLED_ITEM ( 'NONE', ( #3713 ), #16944 ) ;
#6134 = ADVANCED_FACE ( 'NONE', ( #877 ), #6840, .T. ) ;
#6135 = CARTESIAN_POINT ( 'NONE',  ( -83.90000000000000568, -34.81874999877096855, -97.40192378864668399 ) ) ;
#6136 = CARTESIAN_POINT ( 'NONE',  ( -82.39999999999999147, -32.39062499938548001, -96.81714838363319586 ) ) ;
#6137 = LINE ( 'NONE', #1446, #18929 ) ;
#6138 = CARTESIAN_POINT ( 'NONE',  ( 231.2217848218749339, -31.07812499938548001, 102.3871387122750889 ) ) ;
#6139 = CARTESIAN_POINT ( 'NONE',  ( -83.90000000000000568, -32.57268749875867542, 102.5980762113533018 ) ) ;
#6140 = CARTESIAN_POINT ( 'NONE',  ( -81.02178482187500208, -33.70312499938548711, 102.3871387122750889 ) ) ;
#6141 = CARTESIAN_POINT ( 'NONE',  ( -81.02178482187500208, -33.89062499938548711, -102.3871387122750889 ) ) ;
#6142 = CARTESIAN_POINT ( 'NONE',  ( 82.39999999999999147, -32.95312499938548711, 103.1828516163667899 ) ) ;
#6143 = FACE_OUTER_BOUND ( 'NONE', #16668, .T. ) ;
#6144 = PLANE ( 'NONE',  #7705 ) ;
#6145 = CARTESIAN_POINT ( 'NONE',  ( 85.40000000000000568, -35.36739044046696279, -98.90809476984486537 ) ) ;
#6146 = CARTESIAN_POINT ( 'NONE',  ( 232.5999999999999375, -33.71249999999999147, 96.53589838486223584 ) ) ;
#6147 = EDGE_CURVE ( 'NONE', #13275, #13349, #4903, .T. ) ;
#6148 = ORIENTED_EDGE ( 'NONE', *, *, #18134, .F. ) ;
#6149 = CARTESIAN_POINT ( 'NONE',  ( 235.3564303562499447, -32.24062499938548143, -51.59142580818350154 ) ) ;
#6150 = CARTESIAN_POINT ( 'NONE',  ( 0.000000000000000000, 0.000000000000000000, 199.9999999999999716 ) ) ;
#6151 = CARTESIAN_POINT ( 'NONE',  ( 232.5999999999999375, -31.26562499938548356, 96.81714838363319586 ) ) ;
#6152 = EDGE_CURVE ( 'NONE', #13276, #10751, #6468, .T. ) ;
#6153 = CARTESIAN_POINT ( 'NONE',  ( 233.9782151781249411, -30.40312499938547930, -52.38713871227520968 ) ) ;
#6154 = AXIS2_PLACEMENT_3D ( 'NONE', #11208, #13748, #1925 ) ;
#6155 = ADVANCED_FACE ( 'NONE', ( #13158 ), #14876, .F. ) ;
#6156 = CARTESIAN_POINT ( 'NONE',  ( -85.15643035625001289, -32.39062499938548711, 99.99999999999998579 ) ) ;
#6157 = ORIENTED_EDGE ( 'NONE', *, *, #4155, .F. ) ;
#6158 = ORIENTED_EDGE ( 'NONE', *, *, #14769, .F. ) ;
#6159 = CARTESIAN_POINT ( 'NONE',  ( 3.806834918298644954, -3.031088913245539640, 1.750000000000000666 ) ) ;
#6160 =( BOUNDED_CURVE ( )  B_SPLINE_CURVE ( 2, ( #764, #11205, #4168, #2307, #8457, #8271, #9835, #5456, #6717 ),
 .UNSPECIFIED., .F., .F. ) 
 B_SPLINE_CURVE_WITH_KNOTS ( ( 3, 2, 2, 2, 3 ),
 ( 0.5208333333333333703, 0.5277777777777777901, 0.5416666666666666297, 0.5555555555555555802, 0.5625000000000002220 ),
 .UNSPECIFIED. ) 
 CURVE ( )  GEOMETRIC_REPRESENTATION_ITEM ( )  RATIONAL_B_SPLINE_CURVE ( ( 0.9330127018922192983, 0.9330127018922198534, 1.000000000000000000, 0.8660254037844387076, 1.000000000000000000, 0.8660254037844387076, 1.000000000000000000, 0.9330127018922171889, 0.9330127018922194093 ) ) 
 REPRESENTATION_ITEM ( '' )  );
#6161 = CARTESIAN_POINT ( 'NONE',  ( -4.000000000000000000, 1.677772373332757194, -3.535253723897187506 ) ) ;
#6162 = CARTESIAN_POINT ( 'NONE',  ( -83.90000000000000568, -33.97500000000000853, -97.40192378864668399 ) ) ;
#6163 = VERTEX_POINT ( 'NONE', #5941 ) ;
#6164 = PLANE ( 'NONE',  #13877 ) ;
#6165 = CIRCLE ( 'NONE', #4286, 5.200000000000009948 ) ;
#6166 = DIRECTION ( 'NONE',  ( 0.000000000000000000, 1.000000000000000000, 0.000000000000000000 ) ) ;
#6167 = CARTESIAN_POINT ( 'NONE',  ( -81.02178482187500208, -33.55312499938548854, 97.61286128772489690 ) ) ;
#6168 = CARTESIAN_POINT ( 'NONE',  ( -85.40000000000000568, -30.84374999877096712, 99.99999999999998579 ) ) ;
#6169 = CARTESIAN_POINT ( 'NONE',  ( -80.90000000000000568, -31.59374999877097423, 102.5980762113533018 ) ) ;
#6170 = VECTOR ( 'NONE', #6125, 1000.000000000000000 ) ;
#6171 = CARTESIAN_POINT ( 'NONE',  ( 229.5999999999999375, -33.63749999999999574, 98.26794919243111792 ) ) ;
#6172 = DIRECTION ( 'NONE',  ( -0.000000000000000000, -1.000000000000000000, -0.000000000000000000 ) ) ;
#6173 = DIRECTION ( 'NONE',  ( 0.000000000000000000, -0.000000000000000000, -1.000000000000000000 ) ) ;
#6174 = CARTESIAN_POINT ( 'NONE',  ( -80.32125193361316917, -35.00000000000001421, -102.0234471769925193 ) ) ;
#6175 = CARTESIAN_POINT ( 'NONE',  ( 235.3564303562499447, -32.20312499938548001, 101.5914258081833879 ) ) ;
#6176 = VERTEX_POINT ( 'NONE', #13255 ) ;
#6177 = VECTOR ( 'NONE', #16045, 1000.000000000000000 ) ;
#6178 = CARTESIAN_POINT ( 'NONE',  ( -83.77821517812500929, -34.11562499938548854, -97.61286128772489690 ) ) ;
#6179 = CARTESIAN_POINT ( 'NONE',  ( 2.742827927723449299, 3.035229711104609596, -3.433252694550591233 ) ) ;
#6180 = EDGE_CURVE ( 'NONE', #6661, #19103, #17852, .T. ) ;
#6181 = CARTESIAN_POINT ( 'NONE',  ( 94.79999999999995453, -35.00000000000000000, -150.0000000000000000 ) ) ;
#6182 = LINE ( 'NONE', #7536, #3039 ) ;
#6183 = EDGE_CURVE ( 'NONE', #18941, #11625, #14816, .T. ) ;
#6184 = DIRECTION ( 'NONE',  ( 1.000000000000000000, 0.000000000000000000, 0.000000000000000000 ) ) ;
#6185 = AXIS2_PLACEMENT_3D ( 'NONE', #8542, #14399, #9726 ) ;
#6186 = CONICAL_SURFACE ( 'NONE', #18040, 4.000000000000000000, 0.8911886515913786111 ) ;
#6187 = ORIENTED_EDGE ( 'NONE', *, *, #6983, .T. ) ;
#6188 = VERTEX_POINT ( 'NONE', #4375 ) ;
#6189 = CARTESIAN_POINT ( 'NONE',  ( 82.40000000000000568, -34.55624999877097281, 102.9999999999999858 ) ) ;
#6190 = CARTESIAN_POINT ( 'NONE',  ( -82.39999999999999147, -31.46250000000000568, 96.53589838486223584 ) ) ;
#6191 = CARTESIAN_POINT ( 'NONE',  ( -82.39999999999999147, -31.63124999877097210, 103.4641016151377499 ) ) ;
#6192 = CARTESIAN_POINT ( 'NONE',  ( 82.39999999999999147, -31.68750000000000355, 96.53589838486223584 ) ) ;
#6193 = VECTOR ( 'NONE', #13734, 1000.000000000000000 ) ;
#6194 = EDGE_CURVE ( 'NONE', #2988, #17308, #10333, .T. ) ;
#6195 = CARTESIAN_POINT ( 'NONE',  ( 82.40000000000001990, -32.30624999877097281, 103.0000000000000000 ) ) ;
#6196 = CARTESIAN_POINT ( 'NONE',  ( 233.9782151781249411, -33.89062499938548001, 97.61286128772489690 ) ) ;
#6197 = CARTESIAN_POINT ( 'NONE',  ( 79.64356964374998427, -33.14062499938548711, -98.40857419181659793 ) ) ;
#6198 = VECTOR ( 'NONE', #9742, 1000.000000000000000 ) ;
#6199 = CARTESIAN_POINT ( 'NONE',  ( -79.68596062386970402, -32.00000000000002132, -98.72172371342720965 ) ) ;
#6200 = VECTOR ( 'NONE', #10716, 1000.000000000000000 ) ;
#6201 = CARTESIAN_POINT ( 'NONE',  ( 79.64356964374999848, -34.86562499938548143, -99.99999999999998579 ) ) ;
#6202 = ORIENTED_EDGE ( 'NONE', *, *, #13663, .F. ) ;
#6203 = CARTESIAN_POINT ( 'NONE',  ( 235.5999999999999375, -33.37499999999999289, -50.00000000000011369 ) ) ;
#6204 = CARTESIAN_POINT ( 'NONE',  ( -79.39999999999999147, -31.48124999877097352, 98.26794919243110371 ) ) ;
#6205 = CARTESIAN_POINT ( 'NONE',  ( 83.77821517812500929, -32.76562499938548711, -102.3871387122750889 ) ) ;
#6206 = CARTESIAN_POINT ( 'NONE',  ( 232.5999999999999091, -32.08124999877096428, -47.00000000000011369 ) ) ;
#6207 = CARTESIAN_POINT ( 'NONE',  ( -85.15643035624999868, -31.56562499938548427, 101.5914258081833879 ) ) ;
#6208 = CARTESIAN_POINT ( 'NONE',  ( 231.2217848218749339, -33.77812499938547575, -47.61286128772501769 ) ) ;
#6209 = CARTESIAN_POINT ( 'NONE',  ( -82.39999999999999147, -34.75312499938549138, 96.81714838363319586 ) ) ;
#6210 = ORIENTED_EDGE ( 'NONE', *, *, #13630, .F. ) ;
#6211 = CARTESIAN_POINT ( 'NONE',  ( -80.45107360500455229, -35.00092285196230080, 102.2869350179830121 ) ) ;
#6212 = CIRCLE ( 'NONE', #7763, 5.200000000000009948 ) ;
#6213 = CARTESIAN_POINT ( 'NONE',  ( 235.3564303562499447, -34.37812499938547717, 98.40857419181659793 ) ) ;
#6214 = CARTESIAN_POINT ( 'NONE',  ( 85.15643035624999868, -31.07812499938548356, 101.5914258081833879 ) ) ;
#6215 = CARTESIAN_POINT ( 'NONE',  ( -85.40000000000000568, -34.94606250001229597, 99.99999999999998579 ) ) ;
#6216 = CARTESIAN_POINT ( 'NONE',  ( -83.90000000000000568, -33.22500000000000142, -102.5980762113533018 ) ) ;
#6217 = CARTESIAN_POINT ( 'NONE',  ( -79.64356964374998427, -31.34062499938548640, 98.40857419181659793 ) ) ;
#6218 = DIRECTION ( 'NONE',  ( 0.000000000000000000, 0.000000000000000000, -1.000000000000000000 ) ) ;
#6219 = CARTESIAN_POINT ( 'NONE',  ( 85.15643035625001289, -33.85312499938549280, 99.99999999999998579 ) ) ;
#6220 = DIRECTION ( 'NONE',  ( -0.000000000000000000, -1.000000000000000000, -0.000000000000000000 ) ) ;
#6221 = CARTESIAN_POINT ( 'NONE',  ( 234.0999999999999375, -32.84999999999999432, -52.59807621135342970 ) ) ;
#6222 = CARTESIAN_POINT ( 'NONE',  ( -79.64356964374998427, -32.24062499938548854, 98.40857419181659793 ) ) ;
#6223 = CARTESIAN_POINT ( 'NONE',  ( -83.77821517812500929, -34.67812499938548854, -97.61286128772489690 ) ) ;
#6224 = ORIENTED_EDGE ( 'NONE', *, *, #16768, .F. ) ;
#6225 = CARTESIAN_POINT ( 'NONE',  ( 83.77821517812500929, -31.52812499938548996, 97.61286128772489690 ) ) ;
#6226 = FACE_OUTER_BOUND ( 'NONE', #15808, .T. ) ;
#6227 = CARTESIAN_POINT ( 'NONE',  ( 100.0000000000000000, 10.19999999999999396, -150.0000000000000000 ) ) ;
#6228 = CARTESIAN_POINT ( 'NONE',  ( -79.64356964375001269, -32.76562499938548711, 101.5914258081833879 ) ) ;
#6229 = FACE_OUTER_BOUND ( 'NONE', #18073, .T. ) ;
#6230 = ORIENTED_EDGE ( 'NONE', *, *, #13934, .F. ) ;
#6231 = CARTESIAN_POINT ( 'NONE',  ( -82.39999999999999147, -31.01249999999999929, -103.4641016151377499 ) ) ;
#6232 = CARTESIAN_POINT ( 'NONE',  ( 84.69814068649969840, -35.00052333152936512, -98.07164593887567605 ) ) ;
#6233 = CARTESIAN_POINT ( 'NONE',  ( 79.39999999999999147, -33.76874999877097139, 99.99999999999998579 ) ) ;
#6234 = CARTESIAN_POINT ( 'NONE',  ( -85.15643035624999868, -34.26562499938548711, -98.40857419181659793 ) ) ;
#6235 = CARTESIAN_POINT ( 'NONE',  ( 232.5999999999999375, -32.75624999877096144, -53.00000000000010658 ) ) ;
#6236 = CARTESIAN_POINT ( 'NONE',  ( 231.2217848218749339, -33.92812499938548143, 97.61286128772489690 ) ) ;
#6237 = CARTESIAN_POINT ( 'NONE',  ( -85.40000000000000568, -31.74768749875867613, 99.99999999999998579 ) ) ;
#6238 = ORIENTED_EDGE ( 'NONE', *, *, #2545, .F. ) ;
#6239 = FACE_OUTER_BOUND ( 'NONE', #3596, .T. ) ;
#6240 = CARTESIAN_POINT ( 'NONE',  ( 83.90000000000000568, -32.17500000000000426, 97.40192378864668399 ) ) ;
#6241 = CARTESIAN_POINT ( 'NONE',  ( 79.64356964374998427, -34.37812499938548427, 101.5914258081833879 ) ) ;
#6242 = PLANE ( 'NONE',  #11177 ) ;
#6243 = CARTESIAN_POINT ( 'NONE',  ( -84.51155386534844638, -35.25364837475780888, 98.22820752270799005 ) ) ;
#6244 = CARTESIAN_POINT ( 'NONE',  ( 80.90000000000000568, -35.19374999877096855, -102.5980762113533018 ) ) ;
#6245 = CARTESIAN_POINT ( 'NONE',  ( 229.5999999999999375, -33.11249999999999716, 101.7320508075688679 ) ) ;
#6246 = ADVANCED_FACE ( 'NONE', ( #17955 ), #13394, .F. ) ;
#6247 = EDGE_CURVE ( 'NONE', #12925, #10773, #1321, .T. ) ;
#6248 = EDGE_LOOP ( 'NONE', ( #3589, #9100, #12186, #9265, #18364 ) ) ;
#6249 = CARTESIAN_POINT ( 'NONE',  ( 231.2217848218749339, -33.92812499938548143, -52.38713871227520968 ) ) ;
#6250 = DIRECTION ( 'NONE',  ( -1.000000000000000000, 0.000000000000000000, 0.000000000000000000 ) ) ;
#6251 = CARTESIAN_POINT ( 'NONE',  ( 235.5999999999999943, -34.25624999877096855, 101.7320508075688537 ) ) ;
#6252 = CARTESIAN_POINT ( 'NONE',  ( 229.8435696437499871, -30.74062499938547433, -51.59142580818350865 ) ) ;
#6253 = CARTESIAN_POINT ( 'NONE',  ( -84.51155153715826884, -35.14114847181267720, 98.22820474807231506 ) ) ;
#6254 = ORIENTED_EDGE ( 'NONE', *, *, #17204, .F. ) ;
#6255 = ORIENTED_EDGE ( 'NONE', *, *, #7076, .T. ) ;
#6256 = CARTESIAN_POINT ( 'NONE',  ( 229.5999999999999375, -32.68124999877096570, -51.73205080756898866 ) ) ;
#6257 = CARTESIAN_POINT ( 'NONE',  ( -81.59615242270662350, -34.12634618820329990, 96.99999999999998579 ) ) ;
#6258 = CARTESIAN_POINT ( 'NONE',  ( -85.40000000000000568, -34.05000000000000426, -99.99999999999998579 ) ) ;
#6259 = ORIENTED_EDGE ( 'NONE', *, *, #15450, .T. ) ;
#6260 = ADVANCED_FACE ( 'NONE', ( #19196 ), #8771, .F. ) ;
#6261 = DIRECTION ( 'NONE',  ( 1.000000000000000000, 0.000000000000000000, -0.000000000000000000 ) ) ;
#6262 = CARTESIAN_POINT ( 'NONE',  ( 231.0999999999999375, -34.06874999877096144, 97.40192378864668399 ) ) ;
#6263 = EDGE_CURVE ( 'NONE', #19033, #10520, #13693, .T. ) ;
#6264 = CARTESIAN_POINT ( 'NONE',  ( -69.99999999999998579, -32.00000000000000000, 150.0000000000000000 ) ) ;
#6265 = CARTESIAN_POINT ( 'NONE',  ( -85.40000000000000568, -34.46249999999999858, 101.7320508075688679 ) ) ;
#6266 = CARTESIAN_POINT ( 'NONE',  ( -80.90000000000000568, -31.89374999877096784, 97.40192378864668399 ) ) ;
#6267 = CARTESIAN_POINT ( 'NONE',  ( -85.40000000000000568, -30.19687499938548569, 99.99999999999998579 ) ) ;
#6268 = CARTESIAN_POINT ( 'NONE',  ( -85.15643035625001289, -35.16562499938548569, 101.5914258081833879 ) ) ;
#6269 = FILL_AREA_STYLE ('',( #1859 ) ) ;
#6270 = DIRECTION ( 'NONE',  ( 0.000000000000000000, 0.000000000000000000, -1.000000000000000000 ) ) ;
#6271 = DIRECTION ( 'NONE',  ( -0.000000000000000000, -0.000000000000000000, 1.000000000000000000 ) ) ;
#6272 = EDGE_CURVE ( 'NONE', #11529, #5414, #7235, .T. ) ;
#6273 = CARTESIAN_POINT ( 'NONE',  ( 231.2217848218749339, -32.46562499938547575, 97.61286128772489690 ) ) ;
#6274 = ORIENTED_EDGE ( 'NONE', *, *, #17842, .T. ) ;
#6275 = CARTESIAN_POINT ( 'NONE',  ( -81.02178482187500208, -32.09062499938548285, -102.3871387122750889 ) ) ;
#6276 = DIRECTION ( 'NONE',  ( 0.000000000000000000, 0.000000000000000000, 1.000000000000000000 ) ) ;
#6277 =( BOUNDED_CURVE ( )  B_SPLINE_CURVE ( 2, ( #6692, #12635, #18318, #14295, #5617, #2660, #4235, #11752, #11562 ),
 .UNSPECIFIED., .F., .F. ) 
 B_SPLINE_CURVE_WITH_KNOTS ( ( 3, 2, 2, 2, 3 ),
 ( 0.6875000000000000000, 0.6944444444444444198, 0.7083333333333333703, 0.7222222222222222099, 0.7291666666666668517 ),
 .UNSPECIFIED. ) 
 CURVE ( )  GEOMETRIC_REPRESENTATION_ITEM ( )  RATIONAL_B_SPLINE_CURVE ( ( 0.9330127018922194093, 0.9330127018922194093, 1.000000000000000000, 0.8660254037844387076, 1.000000000000000000, 0.8660254037844387076, 1.000000000000000000, 0.9330127018922177440, 0.9330127018922194093 ) ) 
 REPRESENTATION_ITEM ( '' )  );
#6278 = ORIENTED_EDGE ( 'NONE', *, *, #11010, .F. ) ;
#6279 = DIRECTION ( 'NONE',  ( 1.000000000000000000, 0.000000000000000000, 0.000000000000000000 ) ) ;
#6280 = CARTESIAN_POINT ( 'NONE',  ( -83.90000000000000568, -32.71874999877096712, 97.40192378864668399 ) ) ;
#6281 = CARTESIAN_POINT ( 'NONE',  ( 231.3449744686915324, -35.00000000000002842, -47.51146709331043638 ) ) ;
#6282 = DIRECTION ( 'NONE',  ( 0.000000000000000000, -0.000000000000000000, -1.000000000000000000 ) ) ;
#6283 = ORIENTED_EDGE ( 'NONE', *, *, #10207, .F. ) ;
#6284 = ORIENTED_EDGE ( 'NONE', *, *, #12745, .T. ) ;
#6285 = CARTESIAN_POINT ( 'NONE',  ( -84.29633955546275104, -32.00000000000001421, 102.0295751981970511 ) ) ;
#6286 = CARTESIAN_POINT ( 'NONE',  ( 82.39999999999999147, -31.01249999999999929, -96.53589838486223584 ) ) ;
#6287 = CARTESIAN_POINT ( 'NONE',  ( -80.90000000000000568, -31.89374999877096784, 97.40192378864668399 ) ) ;
#6288 = CARTESIAN_POINT ( 'NONE',  ( 80.90000000000000568, -32.40000000000000568, 102.5980762113533018 ) ) ;
#6289 = CARTESIAN_POINT ( 'NONE',  ( 83.20384757729335945, -33.63615380933863008, 102.9999999999999716 ) ) ;
#6290 = CARTESIAN_POINT ( 'NONE',  ( 229.8435696437499303, -33.74062499938548143, 99.99999999999998579 ) ) ;
#6291 = CARTESIAN_POINT ( 'NONE',  ( 85.15643035625001289, -33.44062499938548427, -98.40857419181659793 ) ) ;
#6292 = CARTESIAN_POINT ( 'NONE',  ( 79.58826230851033756, -31.99999999999998579, -98.95399275611669054 ) ) ;
#6293 = CARTESIAN_POINT ( 'NONE',  ( 81.02178482187500208, -32.69062499938548427, -102.3871387122750889 ) ) ;
#6294 = ORIENTED_EDGE ( 'NONE', *, *, #14251, .T. ) ;
#6295 = CARTESIAN_POINT ( 'NONE',  ( 229.5999999999999375, -33.14999999999999147, -50.00000000000011369 ) ) ;
#6296 = CARTESIAN_POINT ( 'NONE',  ( -2.500000000000000888, 0.000000000000000000, -4.974599999999998801 ) ) ;
#6297 = CARTESIAN_POINT ( 'NONE',  ( -85.40000000000000568, -34.50000000000000000, 99.99999999999998579 ) ) ;
#6298 = CYLINDRICAL_SURFACE ( 'NONE', #17256, 3.000000000000002665 ) ;
#6299 = CARTESIAN_POINT ( 'NONE',  ( -79.64356964374999848, -30.47812499938548569, 99.99999999999998579 ) ) ;
#6300 = EDGE_CURVE ( 'NONE', #9376, #2579, #18148, .T. ) ;
#6301 = CARTESIAN_POINT ( 'NONE',  ( 232.5999999999999375, -34.19062499938547717, -46.81714838363331666 ) ) ;
#6302 = CARTESIAN_POINT ( 'NONE',  ( -83.90000000000000568, -30.52500000000000213, 97.40192378864668399 ) ) ;
#6303 = ORIENTED_EDGE ( 'NONE', *, *, #10300, .T. ) ;
#6304 = CARTESIAN_POINT ( 'NONE',  ( -80.17521417250719651, -34.99920530278070885, 97.95730091510780824 ) ) ;
#6305 = CARTESIAN_POINT ( 'NONE',  ( 105.2000000000000739, -32.00000000000002842, 147.7999999999999829 ) ) ;
#6306 = FACE_OUTER_BOUND ( 'NONE', #1659, .T. ) ;
#6307 = VECTOR ( 'NONE', #1205, 1000.000000000000000 ) ;
#6308 = CARTESIAN_POINT ( 'NONE',  ( 84.67508262029679145, -31.99999999999999289, -101.5663513044664938 ) ) ;
#6309 = CARTESIAN_POINT ( 'NONE',  ( -85.15643035625001289, -30.74062499938548143, 98.40857419181659793 ) ) ;
#6310 = CARTESIAN_POINT ( 'NONE',  ( -79.39999999999999147, -32.92500000000000426, 99.99999999999998579 ) ) ;
#6311 = CARTESIAN_POINT ( 'NONE',  ( 79.64356964375001269, -34.94062499938549138, 101.5914258081833879 ) ) ;
#6312 = EDGE_CURVE ( 'NONE', #8719, #9387, #12760, .T. ) ;
#6313 = CARTESIAN_POINT ( 'NONE',  ( 82.39999999999999147, -32.61562499938548854, -96.81714838363319586 ) ) ;
#6314 = CARTESIAN_POINT ( 'NONE',  ( 232.5999999999999375, -30.70312499938548001, -53.18285161636690361 ) ) ;
#6315 = CARTESIAN_POINT ( 'NONE',  ( -85.15643035625001289, -33.85312499938549280, 99.99999999999998579 ) ) ;
#6316 = CARTESIAN_POINT ( 'NONE',  ( -79.64356964375001269, -34.11562499938548854, -98.40857419181659793 ) ) ;
#6317 = PRODUCT_DEFINITION_CONTEXT ( 'detailed design', #14194, 'design' ) ;
#6318 = ORIENTED_EDGE ( 'NONE', *, *, #1048, .F. ) ;
#6319 = CARTESIAN_POINT ( 'NONE',  ( 79.64356964374999848, -30.47812499938548569, 99.99999999999998579 ) ) ;
#6320 = DIRECTION ( 'NONE',  ( 1.000000000000000000, 0.000000000000000000, 0.000000000000000000 ) ) ;
#6321 = CIRCLE ( 'NONE', #17239, 6.000000000000005329 ) ;
#6322 = CARTESIAN_POINT ( 'NONE',  ( -83.20384757729335945, -33.24240381056766580, 96.99999999999998579 ) ) ;
#6323 = AXIS2_PLACEMENT_3D ( 'NONE', #18280, #13484, #9182 ) ;
#6324 = CARTESIAN_POINT ( 'NONE',  ( -79.64356964374999848, -34.52812499938548285, 99.99999999999998579 ) ) ;
#6325 = CARTESIAN_POINT ( 'NONE',  ( -84.44763168836720979, -32.00000000000001421, -98.15470523285542015 ) ) ;
#6326 = ORIENTED_EDGE ( 'NONE', *, *, #8155, .T. ) ;
#6327 = CARTESIAN_POINT ( 'NONE',  ( -80.90000000000000568, -31.20000000000000284, -97.40192378864668399 ) ) ;
#6328 = CARTESIAN_POINT ( 'NONE',  ( 4.050536630291691864, -3.778525289263166442, -0.5912575323401421112 ) ) ;
#6329 = CARTESIAN_POINT ( 'NONE',  ( 85.40000000000000568, -34.85624999877096997, -101.7320508075688821 ) ) ;
#6330 = DIRECTION ( 'NONE',  ( 0.000000000000000000, 1.000000000000000000, 0.000000000000000000 ) ) ;
#6331 = LINE ( 'NONE', #1826, #888 ) ;
#6332 = CARTESIAN_POINT ( 'NONE',  ( 233.9782151781249411, -33.55312499938548143, 97.61286128772489690 ) ) ;
#6333 = CARTESIAN_POINT ( 'NONE',  ( -79.39999999999999147, -34.22268749875867400, 99.99999999999998579 ) ) ;
#6334 = ORIENTED_EDGE ( 'NONE', *, *, #13908, .F. ) ;
#6335 = CARTESIAN_POINT ( 'NONE',  ( -79.64356964375001269, -34.94062499938549138, 98.40857419181659793 ) ) ;
#6336 = CARTESIAN_POINT ( 'NONE',  ( 82.39999999999999147, -32.36250000000000426, 102.9999999999999858 ) ) ;
#6337 = CARTESIAN_POINT ( 'NONE',  ( 81.02178482187500208, -33.14062499938548711, 97.61286128772489690 ) ) ;
#6338 = CARTESIAN_POINT ( 'NONE',  ( 113.0000000000000142, 15.19999999999997442, -150.0000000000000000 ) ) ;
#6339 = VECTOR ( 'NONE', #17827, 1000.000000000000000 ) ;
#6340 = CARTESIAN_POINT ( 'NONE',  ( 82.39999999999999147, -32.81250000000000000, -97.00000000000000000 ) ) ;
#6341 = CARTESIAN_POINT ( 'NONE',  ( 80.90000000000000568, -33.39374999877097139, -102.5980762113533018 ) ) ;
#6342 = DIRECTION ( 'NONE',  ( 0.000000000000000000, 0.000000000000000000, 1.000000000000000000 ) ) ;
#6343 = ORIENTED_EDGE ( 'NONE', *, *, #16183, .T. ) ;
#6344 = CARTESIAN_POINT ( 'NONE',  ( 229.8435696437499587, -32.46562499938548285, -48.40857419181671162 ) ) ;
#6345 = CARTESIAN_POINT ( 'NONE',  ( 231.2217848218749339, -33.47812499938547859, 97.61286128772489690 ) ) ;
#6346 = CARTESIAN_POINT ( 'NONE',  ( 229.8435696437499303, -31.15312499938548285, -50.00000000000011369 ) ) ;
#6347 = CARTESIAN_POINT ( 'NONE',  ( 3.806834918298644066, 3.031088913245536531, -1.749999999999997558 ) ) ;
#6348 = EDGE_LOOP ( 'NONE', ( #2921, #3358, #8211, #16227 ) ) ;
#6349 = ORIENTED_EDGE ( 'NONE', *, *, #5053, .F. ) ;
#6350 = VECTOR ( 'NONE', #4112, 1000.000000000000000 ) ;
#6351 = CARTESIAN_POINT ( 'NONE',  ( -83.20384757729337366, -32.15759618943233278, -97.00000000000000000 ) ) ;
#6352 = ORIENTED_EDGE ( 'NONE', *, *, #17037, .F. ) ;
#6353 = CARTESIAN_POINT ( 'NONE',  ( -82.40000000000000568, -31.18124999877096926, 102.9999999999999858 ) ) ;
#6354 = CLOSED_SHELL ( 'NONE', ( #6749, #1822, #4744, #8034, #18829, #12235, #814, #15320, #3866, #5895, #9215, #7370, #6724, #2200, #1002, #318, #3849, #14658, #14370, #16957, #15924, #15133, #587, #12718, #16400, #6634, #3535, #13764, #7959, #12214, #4012, #11741, #3758, #11062, #17708, #11661, #13242, #18123, #15016, #2674, #5769, #17488, #10444, #14485, #16566, #4722, #4588, #4209, #9849, #5209, #529, #10787, #6729, #7835, #2575, #16518, #17879, #3977, #5943, #8855, #1255, #1593, #1837, #5003, #303, #4387, #17484, #16408, #7802, #15895, #7331, #16275, #5355, #19259, #8436, #3749 ) ) ;
#6355 = CARTESIAN_POINT ( 'NONE',  ( -85.40000000000000568, -32.68124999877097281, -101.7320508075688679 ) ) ;
#6356 = CARTESIAN_POINT ( 'NONE',  ( -2.000000000000007550, -3.464101615137749945, 0.000000000000000000 ) ) ;
#6357 = CARTESIAN_POINT ( 'NONE',  ( -83.90000000000000568, -34.87500000000000000, 102.5980762113533018 ) ) ;
#6358 = CARTESIAN_POINT ( 'NONE',  ( -80.90000000000000568, -33.69374999877096855, 97.40192378864668399 ) ) ;
#6359 = CARTESIAN_POINT ( 'NONE',  ( 110.0000000000000000, 10.19999999999997620, -139.9999999999999716 ) ) ;
#6360 = CARTESIAN_POINT ( 'NONE',  ( -80.90000000000000568, -30.75000000000000355, 102.5980762113533018 ) ) ;
#6361 = CARTESIAN_POINT ( 'NONE',  ( 79.39999999999999147, -34.76250000000000284, -101.7320508075688537 ) ) ;
#6362 = CARTESIAN_POINT ( 'NONE',  ( -79.39999999999999147, -33.33749999999999858, 98.26794919243110371 ) ) ;
#6363 = CARTESIAN_POINT ( 'NONE',  ( 229.8435696437499871, -34.22812499938547148, 98.40857419181659793 ) ) ;
#6364 = B_SPLINE_CURVE_WITH_KNOTS ( 'NONE', 3,
 ( #9570, #17097, #3708, #12693, #3420, #13172, #11427, #17388, #5481, #1269 ),
 .UNSPECIFIED., .F., .F.,
 ( 4, 2, 2, 2, 4 ),
 ( 0.3612006186103786654, 0.3925526867148934063, 0.4239047548194081472, 0.4552568229239228881, 0.4866088910284376290 ),
 .UNSPECIFIED. ) ;
#6365 = CARTESIAN_POINT ( 'NONE',  ( 229.8435696437499871, -31.52812499938547575, 98.40857419181659793 ) ) ;
#6366 = VERTEX_POINT ( 'NONE', #10168 ) ;
#6367 = CARTESIAN_POINT ( 'NONE',  ( -81.02178482187500208, -33.89062499938548711, -102.3871387122750889 ) ) ;
#6368 = CARTESIAN_POINT ( 'NONE',  ( -82.40000000000001990, -32.75624999877096855, -103.0000000000000000 ) ) ;
#6369 = EDGE_LOOP ( 'NONE', ( #17719, #15739, #15622, #12797 ) ) ;
#6370 = DIRECTION ( 'NONE',  ( -1.000000000000000000, 1.586032892321652482E-15, 0.000000000000000000 ) ) ;
#6371 = CARTESIAN_POINT ( 'NONE',  ( 82.40000000000000568, -30.00000000000000355, -99.99999999999998579 ) ) ;
#6372 = CARTESIAN_POINT ( 'NONE',  ( 69.99999999999998579, -31.99999999999998579, -150.0000000000000000 ) ) ;
#6373 = ORIENTED_EDGE ( 'NONE', *, *, #13926, .T. ) ;
#6374 = DIRECTION ( 'NONE',  ( 0.000000000000000000, 0.000000000000000000, -1.000000000000000000 ) ) ;
#6375 = CARTESIAN_POINT ( 'NONE',  ( -82.40000000000001990, -32.13750000000000284, 103.0000000000000000 ) ) ;
#6376 = VERTEX_POINT ( 'NONE', #16677 ) ;
#6377 = CARTESIAN_POINT ( 'NONE',  ( 235.5999999999999943, -33.33749999999999147, -51.73205080756900287 ) ) ;
#6378 = CARTESIAN_POINT ( 'NONE',  ( 79.39999999999999147, -31.08750000000000213, -98.26794919243110371 ) ) ;
#6379 = ADVANCED_FACE ( 'NONE', ( #5774 ), #10272, .F. ) ;
#6380 = CARTESIAN_POINT ( 'NONE',  ( -85.40000000000000568, -34.40624999877096712, 101.7320508075688679 ) ) ;
#6381 = CARTESIAN_POINT ( 'NONE',  ( -85.40000000000000568, -32.23124999877096997, -101.7320508075688821 ) ) ;
#6382 = DIRECTION ( 'NONE',  ( -0.000000000000000000, -1.000000000000000000, -0.000000000000000000 ) ) ;
#6383 = CARTESIAN_POINT ( 'NONE',  ( 81.02178482187500208, -33.10312499938548569, -97.61286128772489690 ) ) ;
#6384 = CARTESIAN_POINT ( 'NONE',  ( 83.52022063337599889, -31.99999999999998579, -97.42682425339255303 ) ) ;
#6385 = CARTESIAN_POINT ( 'NONE',  ( 85.15643035624999868, -34.67812499938548143, -98.40857419181659793 ) ) ;
#6386 = ORIENTED_EDGE ( 'NONE', *, *, #16158, .F. ) ;
#6388 = EDGE_CURVE ( 'NONE', #17929, #7647, #8481, .T. ) ;
#6387 = CARTESIAN_POINT ( 'NONE',  ( 232.5999999999999375, -32.13749999999998863, -46.53589838486234953 ) ) ;
#6389 = CARTESIAN_POINT ( 'NONE',  ( -82.39999999999999147, -34.38750000000000284, 103.4641016151377499 ) ) ;
#6390 = EDGE_CURVE ( 'NONE', #9639, #6735, #3523, .T. ) ;
#6391 = FACE_OUTER_BOUND ( 'NONE', #8561, .T. ) ;
#6392 = CARTESIAN_POINT ( 'NONE',  ( 231.2217848218749339, -32.87812499938547717, 102.3871387122750889 ) ) ;
#6393 = CARTESIAN_POINT ( 'NONE',  ( -79.64356964375001269, -32.31562499938548427, 101.5914258081833879 ) ) ;
#6394 = CARTESIAN_POINT ( 'NONE',  ( 232.5999999999999375, -33.96562499938547575, -53.18285161636690361 ) ) ;
#6395 = EDGE_CURVE ( 'NONE', #2004, #18744, #5534, .T. ) ;
#6396 = CARTESIAN_POINT ( 'NONE',  ( -80.90000000000000568, -31.65000000000000568, 102.5980762113533018 ) ) ;
#6397 = ORIENTED_EDGE ( 'NONE', *, *, #3390, .F. ) ;
#6398 = CARTESIAN_POINT ( 'NONE',  ( -80.32324841350261124, -35.00093580010783256, 102.1718789886361094 ) ) ;
#6399 = DIRECTION ( 'NONE',  ( 0.000000000000000000, 0.000000000000000000, 1.000000000000000000 ) ) ;
#6400 = CARTESIAN_POINT ( 'NONE',  ( 111.5000000000000142, 12.69999999999998508, 50.00000000000001421 ) ) ;
#6401 = CARTESIAN_POINT ( 'NONE',  ( 230.7186334667984227, -32.00000000000000711, -52.01453922190813728 ) ) ;
#6402 = ADVANCED_FACE ( 'NONE', ( #6816 ), #11293, .T. ) ;
#6403 = CARTESIAN_POINT ( 'NONE',  ( -85.15643035625001289, -32.54062499938548569, 98.40857419181659793 ) ) ;
#6404 = CARTESIAN_POINT ( 'NONE',  ( -79.64356964374998427, -32.24062499938548854, -101.5914258081833879 ) ) ;
#6405 = CARTESIAN_POINT ( 'NONE',  ( 83.77821517812500929, -34.67812499938548854, 97.61286128772489690 ) ) ;
#6406 = CARTESIAN_POINT ( 'NONE',  ( 85.15643035624999868, -31.11562499938548854, -101.5914258081833879 ) ) ;
#6407 = CARTESIAN_POINT ( 'NONE',  ( 235.5999999999999375, -32.92499999999999716, -50.00000000000011369 ) ) ;
#6408 = CARTESIAN_POINT ( 'NONE',  ( -82.39999999999999147, -34.19062499938548427, 103.1828516163667899 ) ) ;
#6409 = CARTESIAN_POINT ( 'NONE',  ( -79.64356964375001269, -33.66562499938549280, -98.40857419181659793 ) ) ;
#6410 = EDGE_LOOP ( 'NONE', ( #10331, #14644, #14692, #18934 ) ) ;
#6411 = CARTESIAN_POINT ( 'NONE',  ( 81.02178482187500208, -33.25312499938548427, 97.61286128772489690 ) ) ;
#6412 = CARTESIAN_POINT ( 'NONE',  ( 4.158806965674307854, -1.986429158307096543, -3.559403772175836256 ) ) ;
#6413 = CIRCLE ( 'NONE', #15140, 2.499999999999999556 ) ;
#6414 = CARTESIAN_POINT ( 'NONE',  ( -82.39999999999999147, -33.96562499938548285, 96.81714838363319586 ) ) ;
#6415 = DIRECTION ( 'NONE',  ( 0.000000000000000000, -1.000000000000000000, 0.000000000000000000 ) ) ;
#6416 = ORIENTED_EDGE ( 'NONE', *, *, #4540, .T. ) ;
#6417 = EDGE_CURVE ( 'NONE', #9031, #9797, #12064, .T. ) ;
#6418 = CARTESIAN_POINT ( 'NONE',  ( -85.40000000000000568, -30.48749999999999716, -101.7320508075688679 ) ) ;
#6419 = CARTESIAN_POINT ( 'NONE',  ( 82.39999999999999147, -34.83749999999999858, -103.4641016151377499 ) ) ;
#6420 = CARTESIAN_POINT ( 'NONE',  ( 80.90000000000000568, -33.84374999877096712, 97.40192378864668399 ) ) ;
#6421 = CARTESIAN_POINT ( 'NONE',  ( -96.99999999999998579, -5.200000000000000178, -150.0000000000000000 ) ) ;
#6422 = CARTESIAN_POINT ( 'NONE',  ( 229.5999999999999375, -33.05624999877096570, -48.26794919243123161 ) ) ;
#6423 = CARTESIAN_POINT ( 'NONE',  ( 235.3564303562499447, -35.01562499938548001, 101.5914258081833879 ) ) ;
#6424 = CARTESIAN_POINT ( 'NONE',  ( -85.40000000000000568, -33.06018749875867258, 101.7320508075688679 ) ) ;
#6425 = ORIENTED_EDGE ( 'NONE', *, *, #8908, .F. ) ;
#6426 = ADVANCED_FACE ( 'NONE', ( #15602 ), #16872, .F. ) ;
#6427 = PRODUCT_DEFINITION ( 'UNKNOWN', '', #7075, #270 ) ;
#6428 = CARTESIAN_POINT ( 'NONE',  ( 105.1999999999999744, -31.99999999999999289, -100.0000000000000000 ) ) ;
#6429 = CARTESIAN_POINT ( 'NONE',  ( 82.40000000000000568, -34.61250000000001137, -97.00000000000000000 ) ) ;
#6430 = CARTESIAN_POINT ( 'NONE',  ( -83.90000000000000568, -33.61874999877097281, -102.5980762113533018 ) ) ;
#6431 = CYLINDRICAL_SURFACE ( 'NONE', #16178, 5.199999999999996625 ) ;
#6432 = VECTOR ( 'NONE', #163, 1000.000000000000000 ) ;
#6433 = CARTESIAN_POINT ( 'NONE',  ( -85.40000000000000568, -30.00000000000000355, 99.99999999999998579 ) ) ;
#6434 = CARTESIAN_POINT ( 'NONE',  ( 79.64356964375001269, -32.31562499938548427, -101.5914258081833879 ) ) ;
#6435 = CARTESIAN_POINT ( 'NONE',  ( 79.39999999999999147, -34.76250000000000284, 98.26794919243113213 ) ) ;
#6436 = ORIENTED_EDGE ( 'NONE', *, *, #5054, .T. ) ;
#6437 = CARTESIAN_POINT ( 'NONE',  ( 233.9782151781249411, -32.80312499938548143, -47.61286128772501769 ) ) ;
#6438 = APPLICATION_PROTOCOL_DEFINITION ( 'draft international standard', 'automotive_design', 1998, #94 ) ;
#6439 = CARTESIAN_POINT ( 'NONE',  ( 235.3564303562499447, -31.82812499938547646, 99.99999999999998579 ) ) ;
#6440 = CARTESIAN_POINT ( 'NONE',  ( 232.5999999999999375, -31.04062499938547859, -46.81714838363331666 ) ) ;
#6441 = CARTESIAN_POINT ( 'NONE',  ( -82.39999999999999147, -34.07812499938548711, 103.1828516163667899 ) ) ;
#6442 = CARTESIAN_POINT ( 'NONE',  ( 111.0000000000000000, 10.19999999999997620, -142.6499999999999773 ) ) ;
#6443 = ORIENTED_EDGE ( 'NONE', *, *, #9010, .F. ) ;
#6444 = ORIENTED_EDGE ( 'NONE', *, *, #6194, .F. ) ;
#6445 = CARTESIAN_POINT ( 'NONE',  ( 3.951447005078450037, -2.357513599190973252, 2.916666666666666963 ) ) ;
#6446 = CIRCLE ( 'NONE', #13917, 6.000000000000005329 ) ;
#6447 = CARTESIAN_POINT ( 'NONE',  ( -85.40000000000000568, -30.84374999877096712, 99.99999999999998579 ) ) ;
#6448 = CARTESIAN_POINT ( 'NONE',  ( -85.40000000000000568, -33.60000000000000142, -99.99999999999998579 ) ) ;
#6449 = EDGE_LOOP ( 'NONE', ( #2140, #994, #2516, #4904 ) ) ;
#6450 = DIRECTION ( 'NONE',  ( -1.000000000000000000, 1.387778780781445676E-15, 2.407412430484046130E-31 ) ) ;
#6451 = CARTESIAN_POINT ( 'NONE',  ( -79.39999999999999147, -34.66874999877096997, -99.99999999999998579 ) ) ;
#6452 = DIRECTION ( 'NONE',  ( 0.000000000000000000, 1.000000000000000000, 0.000000000000000000 ) ) ;
#6453 = CARTESIAN_POINT ( 'NONE',  ( -79.39999999999999147, -32.83124999877097139, 98.26794919243110371 ) ) ;
#6454 = CARTESIAN_POINT ( 'NONE',  ( -83.90000000000000568, -33.91874999877096997, 102.5980762113533018 ) ) ;
#6455 = CARTESIAN_POINT ( 'NONE',  ( -79.39999999999999147, -30.61874999877096926, 99.99999999999998579 ) ) ;
#6456 = CARTESIAN_POINT ( 'NONE',  ( 235.5999999999999375, -32.41874999877096286, 99.99999999999998579 ) ) ;
#6457 = DIRECTION ( 'NONE',  ( 0.000000000000000000, -0.000000000000000000, -1.000000000000000000 ) ) ;
#6458 = CARTESIAN_POINT ( 'NONE',  ( 233.9782151781249411, -33.14062499938548001, 102.3871387122750889 ) ) ;
#6459 = ORIENTED_EDGE ( 'NONE', *, *, #7602, .F. ) ;
#6460 = CARTESIAN_POINT ( 'NONE',  ( 231.0999999999999375, -30.91874999877096286, 97.40192378864668399 ) ) ;
#6461 = CARTESIAN_POINT ( 'NONE',  ( 4.175075985190097150, 4.120741555260244660, 1.921191574886163109E-14 ) ) ;
#6462 = EDGE_LOOP ( 'NONE', ( #12193, #10512, #15866, #9856 ) ) ;
#6463 = CARTESIAN_POINT ( 'NONE',  ( -79.39999999999999147, -33.37500000000000000, -99.99999999999998579 ) ) ;
#6464 = UNCERTAINTY_MEASURE_WITH_UNIT (LENGTH_MEASURE( 1.000000000000000082E-05 ), #8973, 'distance_accuracy_value', 'NONE');
#6465 = VECTOR ( 'NONE', #9875, 1000.000000000000000 ) ;
#6466 = CARTESIAN_POINT ( 'NONE',  ( 0.000000000000000000, 0.000000000000000000, 0.000000000000000000 ) ) ;
#6467 = ORIENTED_EDGE ( 'NONE', *, *, #9613, .F. ) ;
#6468 = B_SPLINE_CURVE_WITH_KNOTS ( 'NONE', 3,
 ( #4278, #7497, #8767, #5747, #19129, #14717 ),
 .UNSPECIFIED., .F., .F.,
 ( 4, 2, 4 ),
 ( 0.01308430721348208606, 0.01410661710602281044, 0.01512892699856353655 ),
 .UNSPECIFIED. ) ;
#6469 = CARTESIAN_POINT ( 'NONE',  ( 229.5999999999999375, -33.54374999877096286, 99.99999999999998579 ) ) ;
#6470 = EDGE_LOOP ( 'NONE', ( #10369, #9384, #18366, #12328 ) ) ;
#6471 = EDGE_LOOP ( 'NONE', ( #17015, #13132, #850, #11070 ) ) ;
#6472 = CARTESIAN_POINT ( 'NONE',  ( 81.59615242270662350, -33.22634618820330843, -97.00000000000000000 ) ) ;
#6473 = CARTESIAN_POINT ( 'NONE',  ( 85.15643035625001289, -35.09062499938548285, -99.99999999999998579 ) ) ;
#6474 = CARTESIAN_POINT ( 'NONE',  ( -85.40000000000000568, -30.43124999877096926, 98.26794919243111792 ) ) ;
#6475 = VECTOR ( 'NONE', #11498, 1000.000000000000000 ) ;
#6476 = CARTESIAN_POINT ( 'NONE',  ( -79.39999999999999147, -33.35624999877097707, 101.7320508075688537 ) ) ;
#6477 = CARTESIAN_POINT ( 'NONE',  ( -82.40000000000000568, -32.30624999877097281, -102.9999999999999858 ) ) ;
#6478 = CARTESIAN_POINT ( 'NONE',  ( -3.355112389629170799, 2.681727112203152963, -0.2256878752776689534 ) ) ;
#6479 = CARTESIAN_POINT ( 'NONE',  ( 79.64356964374998427, -34.04062499938549280, -98.40857419181659793 ) ) ;
#6480 = AXIS2_PLACEMENT_3D ( 'NONE', #16628, #2854, #10571 ) ;
#6481 = CARTESIAN_POINT ( 'NONE',  ( -82.40000000000000568, -30.00000000000000355, 99.99999999999998579 ) ) ;
#6482 = CARTESIAN_POINT ( 'NONE',  ( -81.02178482187500208, -33.89062499938548711, 97.61286128772489690 ) ) ;
#6483 = CARTESIAN_POINT ( 'NONE',  ( 82.39999999999999147, -33.17812499938548854, -103.1828516163667899 ) ) ;
#6484 = VERTEX_POINT ( 'NONE', #17163 ) ;
#6485 = CARTESIAN_POINT ( 'NONE',  ( 229.5999999999999375, -33.18749999999999289, -51.73205080756898866 ) ) ;
#6486 = CARTESIAN_POINT ( 'NONE',  ( -85.40000000000000568, -33.60000000000000142, 99.99999999999998579 ) ) ;
#6487 = AXIS2_PLACEMENT_3D ( 'NONE', #2891, #12167, #8847 ) ;
#6488 = ADVANCED_FACE ( 'NONE', ( #17261 ), #16964, .F. ) ;
#6489 = EDGE_CURVE ( 'NONE', #6967, #15345, #2116, .T. ) ;
#6490 = CARTESIAN_POINT ( 'NONE',  ( -85.40000000000000568, -30.90000000000000213, 99.99999999999998579 ) ) ;
#6491 = CARTESIAN_POINT ( 'NONE',  ( 231.2217848218749339, -32.42812499938548143, 102.3871387122750889 ) ) ;
#6492 = CARTESIAN_POINT ( 'NONE',  ( -79.64356964375001269, -31.79062499938548569, 98.40857419181659793 ) ) ;
#6493 = CARTESIAN_POINT ( 'NONE',  ( 233.9782151781249411, -33.25312499938547717, -47.61286128772501769 ) ) ;
#6494 = CARTESIAN_POINT ( 'NONE',  ( -83.90000000000000568, -33.22500000000000142, 97.40192378864668399 ) ) ;
#6495 = ORIENTED_EDGE ( 'NONE', *, *, #14345, .F. ) ;
#6496 = CARTESIAN_POINT ( 'NONE',  ( -84.70388354820684640, -35.00002705695768412, 98.07851859032987818 ) ) ;
#6497 = AXIS2_PLACEMENT_3D ( 'NONE', #3718, #7922, #8015 ) ;
#6498 = CARTESIAN_POINT ( 'NONE',  ( 233.4038475772933054, -33.73259618943232852, -53.00000000000010658 ) ) ;
#6499 = CARTESIAN_POINT ( 'NONE',  ( 81.02178482187500208, -32.99062499938548854, 102.3871387122750889 ) ) ;
#6500 = AXIS2_PLACEMENT_3D ( 'NONE', #11549, #19073, #3927 ) ;
#6501 = AXIS2_PLACEMENT_3D ( 'NONE', #10295, #14387, #13118 ) ;
#6502 = EDGE_CURVE ( 'NONE', #11363, #9425, #18731, .T. ) ;
#6503 = CARTESIAN_POINT ( 'NONE',  ( 79.58826230851033756, -31.99999999999998579, -98.95399275611669054 ) ) ;
#6504 = EDGE_CURVE ( 'NONE', #19154, #4909, #6908, .T. ) ;
#6505 = CARTESIAN_POINT ( 'NONE',  ( -83.77821517812500929, -31.22812499938548569, 97.61286128772489690 ) ) ;
#6506 = CARTESIAN_POINT ( 'NONE',  ( -85.15643035625001289, -32.46562499938548996, -98.40857419181659793 ) ) ;
#6507 = CARTESIAN_POINT ( 'NONE',  ( 79.64356964374999848, -34.52812499938548285, 99.99999999999998579 ) ) ;
#6508 = CARTESIAN_POINT ( 'NONE',  ( 85.15643035624999868, -31.56562499938548427, -101.5914258081833879 ) ) ;
#6509 = VECTOR ( 'NONE', #17930, 1000.000000000000114 ) ;
#6510 = CARTESIAN_POINT ( 'NONE',  ( 231.2217848218749339, -31.11562499938547788, -52.38713871227520968 ) ) ;
#6511 = CARTESIAN_POINT ( 'NONE',  ( -82.39999999999999147, -34.64062499938548711, 103.1828516163667899 ) ) ;
#6512 = CARTESIAN_POINT ( 'NONE',  ( -82.39999999999999147, -33.51562499938548001, -103.1828516163667899 ) ) ;
#6513 = ORIENTED_EDGE ( 'NONE', *, *, #11389, .T. ) ;
#6514 = CARTESIAN_POINT ( 'NONE',  ( 82.39999999999999147, -32.16562499938549280, 103.1828516163667899 ) ) ;
#6515 = CARTESIAN_POINT ( 'NONE',  ( 229.5999999999999375, -32.24999999999999289, 99.99999999999998579 ) ) ;
#6516 = AXIS2_PLACEMENT_3D ( 'NONE', #10366, #11548, #14757 ) ;
#6517 = DIRECTION ( 'NONE',  ( -1.000000000000000000, 1.156482317317870344E-15, 0.000000000000000000 ) ) ;
#6518 = CARTESIAN_POINT ( 'NONE',  ( -82.39999999999999147, -34.41562499938547859, 96.81714838363319586 ) ) ;
#6519 = CARTESIAN_POINT ( 'NONE',  ( 232.5999999999999659, -32.13749999999999574, -47.00000000000011369 ) ) ;
#6520 = ORIENTED_EDGE ( 'NONE', *, *, #8170, .T. ) ;
#6521 = CARTESIAN_POINT ( 'NONE',  ( -79.39999999999999147, -32.92500000000000426, -99.99999999999998579 ) ) ;
#6522 = CARTESIAN_POINT ( 'NONE',  ( 3.511755186886750923, -2.826662030176382956, -3.597382984111582083 ) ) ;
#6523 = CARTESIAN_POINT ( 'NONE',  ( -82.40000000000000568, -30.00000000000000355, 99.99999999999998579 ) ) ;
#6524 = CARTESIAN_POINT ( 'NONE',  ( -85.15643035624999868, -35.16562499938547859, -98.40857419181659793 ) ) ;
#6525 = CARTESIAN_POINT ( 'NONE',  ( 233.9782151781249411, -34.00312499938547717, 97.61286128772489690 ) ) ;
#6526 = CARTESIAN_POINT ( 'NONE',  ( -85.40000000000000568, -34.93518749875867968, 98.26794919243111792 ) ) ;
#6527 = ORIENTED_EDGE ( 'NONE', *, *, #14610, .F. ) ;
#6528 = CARTESIAN_POINT ( 'NONE',  ( -82.40000000000000568, -30.00000000000000355, 99.99999999999998579 ) ) ;
#6529 = DIRECTION ( 'NONE',  ( -1.000000000000000000, -0.000000000000000000, -0.000000000000000000 ) ) ;
#6530 = PLANE ( 'NONE',  #15165 ) ;
#6531 = CARTESIAN_POINT ( 'NONE',  ( 82.40000000000001990, -34.16250000000000853, 103.0000000000000000 ) ) ;
#6532 = DIRECTION ( 'NONE',  ( 0.000000000000000000, 0.000000000000000000, -1.000000000000000000 ) ) ;
#6533 = CARTESIAN_POINT ( 'NONE',  ( 82.39999999999999147, -31.71562499938548640, -96.81714838363319586 ) ) ;
#6534 = DIRECTION ( 'NONE',  ( 1.000000000000000000, 0.000000000000000000, 0.000000000000000000 ) ) ;
#6535 = ORIENTED_EDGE ( 'NONE', *, *, #12971, .T. ) ;
#6536 = CARTESIAN_POINT ( 'NONE',  ( 229.8435696437499303, -34.75312499938547717, -50.00000000000011369 ) ) ;
#6537 = CARTESIAN_POINT ( 'NONE',  ( 232.5999999999999375, -31.71562499938547930, 96.81714838363319586 ) ) ;
#6538 = CARTESIAN_POINT ( 'NONE',  ( 232.5999999999999375, -31.71562499938547930, -53.18285161636690361 ) ) ;
#6539 = CARTESIAN_POINT ( 'NONE',  ( -85.15643035624999868, -32.42812499938548854, 98.40857419181659793 ) ) ;
#6540 = CARTESIAN_POINT ( 'NONE',  ( -85.40000000000000568, -34.95000000000000284, 99.99999999999998579 ) ) ;
#6541 = EDGE_LOOP ( 'NONE', ( #3759, #5628, #1847, #4935 ) ) ;
#6543 = VERTEX_POINT ( 'NONE', #12467 ) ;
#6542 = EDGE_CURVE ( 'NONE', #6661, #12219, #8171, .T. ) ;
#6544 = CARTESIAN_POINT ( 'NONE',  ( -85.15643035625001289, -30.59062499938548285, -99.99999999999998579 ) ) ;
#6545 = DIRECTION ( 'NONE',  ( -0.000000000000000000, 0.000000000000000000, -1.000000000000000000 ) ) ;
#6546 = CARTESIAN_POINT ( 'NONE',  ( -94.79999999999999716, -5.200000000000000178, 150.0000000000000000 ) ) ;
#6547 = ORIENTED_EDGE ( 'NONE', *, *, #13345, .T. ) ;
#6548 = CARTESIAN_POINT ( 'NONE',  ( -83.20384757729337366, -31.20134618820330630, 102.9999999999999858 ) ) ;
#6549 = CARTESIAN_POINT ( 'NONE',  ( -85.40000000000000568, -33.05624999877096570, -98.26794919243111792 ) ) ;
#6550 = DIRECTION ( 'NONE',  ( 1.000000000000000000, -1.387778780781445478E-15, -2.407412430484046130E-31 ) ) ;
#6551 = CARTESIAN_POINT ( 'NONE',  ( -80.90000000000000568, -31.14374999877097139, 102.5980762113533018 ) ) ;
#6552 =( BOUNDED_CURVE ( )  B_SPLINE_CURVE ( 2, ( #3432, #7923, #4617, #13873, #14968, #16537, #1682, #13497, #6086 ),
 .UNSPECIFIED., .F., .F. ) 
 B_SPLINE_CURVE_WITH_KNOTS ( ( 3, 2, 2, 2, 3 ),
 ( 0.5625000000000000000, 0.5694444444444444198, 0.5833333333333333703, 0.5972222222222222099, 0.6041666666666666297 ),
 .UNSPECIFIED. ) 
 CURVE ( )  GEOMETRIC_REPRESENTATION_ITEM ( )  RATIONAL_B_SPLINE_CURVE ( ( 0.9330127018922194093, 0.9330127018922194093, 1.000000000000000000, 0.8660254037844387076, 1.000000000000000000, 0.8660254037844387076, 1.000000000000000000, 0.9330127018922198534, 0.9330127018922192983 ) ) 
 REPRESENTATION_ITEM ( '' )  );
#6553 = CARTESIAN_POINT ( 'NONE',  ( -85.40000000000000568, -33.58124999877097139, 98.26794919243111792 ) ) ;
#6554 = CARTESIAN_POINT ( 'NONE',  ( 3.973110223767137850, 2.263313079739336463E-11, 3.565797985667434222 ) ) ;
#6555 = CARTESIAN_POINT ( 'NONE',  ( 82.39999999999999147, -34.33124999877097139, -103.0000000000000000 ) ) ;
#6556 = CARTESIAN_POINT ( 'NONE',  ( 232.5999999999999375, -33.48749999999999716, 103.0000000000000000 ) ) ;
#6557 = CARTESIAN_POINT ( 'NONE',  ( 235.3564303562499447, -34.41562499938547859, 99.99999999999998579 ) ) ;
#6558 = ORIENTED_EDGE ( 'NONE', *, *, #161, .T. ) ;
#6559 = CARTESIAN_POINT ( 'NONE',  ( -83.77821517812500929, -34.56562499938548427, -97.61286128772489690 ) ) ;
#6560 = CARTESIAN_POINT ( 'NONE',  ( -79.39999999999999147, -32.90624999877096712, -98.26794919243113213 ) ) ;
#6561 = ORIENTED_EDGE ( 'NONE', *, *, #9238, .T. ) ;
#6562 = CARTESIAN_POINT ( 'NONE',  ( -85.40000000000000568, -33.50624999877096855, 101.7320508075688821 ) ) ;
#6563 = DIRECTION ( 'NONE',  ( 0.000000000000000000, -1.000000000000000000, 3.597944987211154374E-15 ) ) ;
#6564 = CARTESIAN_POINT ( 'NONE',  ( -82.40000000000000568, -30.00000000000000355, 99.99999999999998579 ) ) ;
#6565 = EDGE_LOOP ( 'NONE', ( #18458, #18721, #3216, #13563, #17910, #5657, #13683, #12420, #1787, #8896, #8781, #18194, #8983, #11654, #1627, #15064, #12707, #15179, #15201, #11116, #149, #4590, #612, #4305, #2451 ) ) ;
#6566 = CARTESIAN_POINT ( 'NONE',  ( 231.2217848218749339, -34.26562499938548001, -52.38713871227520968 ) ) ;
#6567 = CARTESIAN_POINT ( 'NONE',  ( 235.5999999999999943, -33.80624999877096570, -48.26794919243124582 ) ) ;
#6568 = ORIENTED_EDGE ( 'NONE', *, *, #10099, .T. ) ;
#6569 = CARTESIAN_POINT ( 'NONE',  ( 235.5999999999999943, -33.41249999999999432, -48.26794919243124582 ) ) ;
#6570 = CARTESIAN_POINT ( 'NONE',  ( 85.15643035624999868, -34.67812499938548143, -98.40857419181659793 ) ) ;
#6571 = CARTESIAN_POINT ( 'NONE',  ( -5.560781378645575757, 6.809993116116508640E-16, -4.000000000000000000 ) ) ;
#6572 = CARTESIAN_POINT ( 'NONE',  ( -85.15643035624999868, -30.29062499938548925, 98.40857419181659793 ) ) ;
#6573 = CARTESIAN_POINT ( 'NONE',  ( -85.40000000000000568, -34.53356250001228744, 98.26794919243111792 ) ) ;
#6574 = CARTESIAN_POINT ( 'NONE',  ( 85.40000000000000568, -32.28750000000000142, -98.26794919243111792 ) ) ;
#6575 = CARTESIAN_POINT ( 'NONE',  ( 232.5999999999999375, -29.99999999999999645, -53.00000000000012079 ) ) ;
#6576 = CARTESIAN_POINT ( 'NONE',  ( 85.15643035625001289, -34.26562499938548711, -101.5914258081833879 ) ) ;
#6577 = CARTESIAN_POINT ( 'NONE',  ( -79.39999999999999147, -33.37500000000000000, 99.99999999999998579 ) ) ;
#6578 = CARTESIAN_POINT ( 'NONE',  ( -85.15643035625001289, -33.74062499938548854, 99.99999999999998579 ) ) ;
#6579 = EDGE_CURVE ( 'NONE', #540, #2299, #17624, .T. ) ;
#6580 =( BOUNDED_CURVE ( )  B_SPLINE_CURVE ( 2, ( #14460, #14181, #6961, #12621, #3924, #2264, #4120, #2546, #15945 ),
 .UNSPECIFIED., .F., .F. ) 
 B_SPLINE_CURVE_WITH_KNOTS ( ( 3, 2, 2, 2, 3 ),
 ( 0.3125000000000000555, 0.3194444444444444198, 0.3333333333333333148, 0.3472222222222222099, 0.3541666666666666852 ),
 .UNSPECIFIED. ) 
 CURVE ( )  GEOMETRIC_REPRESENTATION_ITEM ( )  RATIONAL_B_SPLINE_CURVE ( ( 0.9330127018922192983, 0.9330127018922198534, 1.000000000000000000, 0.8660254037844387076, 1.000000000000000000, 0.8660254037844387076, 1.000000000000000000, 0.9330127018922190762, 0.9330127018922194093 ) ) 
 REPRESENTATION_ITEM ( '' )  );
#6581 = CARTESIAN_POINT ( 'NONE',  ( 79.64356964375001269, -33.55312499938548854, -101.5914258081833879 ) ) ;
#6582 = EDGE_LOOP ( 'NONE', ( #7515, #6831, #7449, #4622 ) ) ;
#6583 = CARTESIAN_POINT ( 'NONE',  ( 82.40000000000000568, -33.03750000000000142, 96.99999999999998579 ) ) ;
#6584 = CARTESIAN_POINT ( 'NONE',  ( -83.90000000000000568, -33.67500000000000426, 97.40192378864668399 ) ) ;
#6585 = CARTESIAN_POINT ( 'NONE',  ( 85.40000000000000568, -33.50624999877096855, -101.7320508075688821 ) ) ;
#6586 = CARTESIAN_POINT ( 'NONE',  ( 235.3564303562499447, -32.76562499938548001, 101.5914258081833879 ) ) ;
#6587 = CARTESIAN_POINT ( 'NONE',  ( -83.77821517812500929, -31.07812499938548711, 102.3871387122750889 ) ) ;
#6588 = CARTESIAN_POINT ( 'NONE',  ( 235.3564303562499447, -34.07812499938548001, -50.00000000000011369 ) ) ;
#6589 = CARTESIAN_POINT ( 'NONE',  ( -79.39999999999999147, -32.51250000000000284, 101.7320508075688537 ) ) ;
#6590 = VERTEX_POINT ( 'NONE', #1422 ) ;
#6591 =( REPRESENTATION_RELATIONSHIP ('NONE','NONE', #14468, #16991 ) REPRESENTATION_RELATIONSHIP_WITH_TRANSFORMATION ( #18936 )SHAPE_REPRESENTATION_RELATIONSHIP( ) );
#6592 = CARTESIAN_POINT ( 'NONE',  ( 4.033906725094790424, -1.419670120618843789, 3.500000000000000888 ) ) ;
#6593 = DIRECTION ( 'NONE',  ( -0.000000000000000000, -1.000000000000000000, -0.000000000000000000 ) ) ;
#6594 = CARTESIAN_POINT ( 'NONE',  ( 82.39999999999999147, -31.37812499938548427, 96.81714838363319586 ) ) ;
#6595 = CARTESIAN_POINT ( 'NONE',  ( 84.93334430221544551, -31.99999999999998579, -101.1009827666102581 ) ) ;
#6596 = CARTESIAN_POINT ( 'NONE',  ( -79.64356964374998427, -31.41562499938548569, 101.5914258081833879 ) ) ;
#6597 = CARTESIAN_POINT ( 'NONE',  ( -85.15643035625001289, -32.54062499938548569, -101.5914258081833879 ) ) ;
#6598 = CARTESIAN_POINT ( 'NONE',  ( 83.77821517812500929, -33.36562499938548854, 102.3871387122750889 ) ) ;
#6599 = CARTESIAN_POINT ( 'NONE',  ( 81.02178482187500208, -32.20312499938548711, -97.61286128772489690 ) ) ;
#6600 = FACE_OUTER_BOUND ( 'NONE', #16430, .T. ) ;
#6601 = CARTESIAN_POINT ( 'NONE',  ( -81.02178482187500208, -34.90312499938548285, 97.61286128772489690 ) ) ;
#6602 = CARTESIAN_POINT ( 'NONE',  ( -82.39999999999999147, -33.06562499938548427, -103.1828516163667899 ) ) ;
#6603 = EDGE_LOOP ( 'NONE', ( #6373, #11688, #306 ) ) ;
#6604 = CARTESIAN_POINT ( 'NONE',  ( 82.39999999999999147, -33.29062499938549280, 96.81714838363319586 ) ) ;
#6605 = FACE_OUTER_BOUND ( 'NONE', #1420, .T. ) ;
#6606 = CARTESIAN_POINT ( 'NONE',  ( -79.64356964374999848, -30.81562499938548427, 99.99999999999998579 ) ) ;
#6607 = CARTESIAN_POINT ( 'NONE',  ( -82.39999999999999147, -34.86562499938548854, 96.81714838363319586 ) ) ;
#6608 = EDGE_CURVE ( 'NONE', #6061, #8383, #8087, .T. ) ;
#6609 = DIRECTION ( 'NONE',  ( 0.000000000000000000, 0.000000000000000000, -1.000000000000000000 ) ) ;
#6610 = ORIENTED_EDGE ( 'NONE', *, *, #17833, .T. ) ;
#6611 = CARTESIAN_POINT ( 'NONE',  ( -85.40000000000000568, -34.08749999999999858, -101.7320508075688679 ) ) ;
#6612 =( BOUNDED_SURFACE ( )  B_SPLINE_SURFACE ( 1, 2, ( 
 ( #12817, #14851, #23, #1475, #7433, #16708, #8890, #13390, #7622, #213, #12018, #4502, #3124, #11830, #316, #14755, #2938, #3032, #17990, #5973, #13575, #10648, #9081, #3221, #11923, #5880, #18090, #15143, #1760, #7717, #13677, #8799, #6169, #18181, #12120, #4699, #17797, #17894, #1387, #8991, #6266, #122, #4407, #16328, #10458, #13287, #10364, #12211, #16421, #10560, #4602, #16521, #14953, #19262, #1578, #7335, #7526, #6073, #13482, #4804, #15047, #16615, #1670, #9179, #10744, #11228, #16995, #4996, #12595, #3606, #16905, #4894, #789, #11125, #9567, #501, #9370, #13859, #15332, #1951, #3317, #3418, #7909, #2151, #14061, #6553, #18377, #15534, #6358, #14155, #9275, #16810, #3511, #12498, #6454, #8108, #5180, #696, #17093, #12406, #410, #18563, #9672, #15633, #2238, #8206, #15242, #6650, #12691, #3706, #10938, #9471, #6744, #18664, #1856, #18468, #18277, #5283, #7814, #13770, #12310, #10838, #15433, #2046, #8005, #13961, #604, #5088, #11031, #6936, #14247, #7213, #1070, #885, #12887 ),
 ( #8297, #10149, #3998, #16111, #18858, #13167, #15824, #18952, #5575, #11522, #8479, #8392, #3797, #3896, #14343, #10054, #7124, #12981, #1166, #9963, #2333, #17578, #14631, #17483, #4189, #4092, #5478, #16014, #2719, #17193, #2522, #14533, #9863, #6846, #11424, #981, #8678, #19043, #17385, #12791, #1266, #2617, #18760, #15917, #5379, #14436, #11327, #13077, #17292, #7027, #8578, #5666, #11609, #2433, #19138, #5755, #9766, #15728, #9059, #10625, #1451, #3005, #12091, #7404, #15024, #11807, #16590, #2914, #1362, #10431, #1555, #14726, #13459, #4572, #190, #11896, #13648, #8866, #1644, #10251, #15117, #14824, #16395, #6047, #5854, #13550, #1733, #7503, #13367, #1, #4287, #7691, #6140, #288, #17776, #5949, #17867, #3195, #11705, #17673, #16213, #16497, #4478, #4383, #18064, #95, #7597, #8963, #11994, #2819, #4675, #14930, #9154, #8776, #7306, #13263, #10340, #19237, #17962, #16304, #10530, #3100, #15506, #12474, #18537, #6335, #14125, #2215, #3582, #9541, #5153, #13935, #8178, #18442, #3289 ) ),
 .UNSPECIFIED., .F., .F., .F. ) 
 B_SPLINE_SURFACE_WITH_KNOTS ( ( 2, 2 ),
 ( 3, 2, 2, 2, 2, 2, 2, 2, 2, 2, 2, 2, 2, 2, 2, 2, 2, 2, 2, 2, 2, 2, 2, 2, 2, 2, 2, 2, 2, 2, 2, 2, 2, 2, 2, 2, 2, 2, 2, 2, 2, 2, 2, 2, 2, 2, 2, 2, 2, 2, 2, 2, 2, 2, 2, 2, 2, 2, 2, 2, 2, 2, 2, 2, 2, 2, 2, 3 ),
 ( 0.000000000000000000, 1.000000000000000000 ),
 ( 0.000000000000000000, 0.01388888888888888812, 0.02777777777777777624, 0.04166666666666666435, 0.05555555555555555247, 0.06944444444444444753, 0.08333333333333332871, 0.09722222222222222376, 0.1111111111111111049, 0.1250000000000000000, 0.1388888888888888951, 0.1527777777777777901, 0.1666666666666666574, 0.1805555555555555525, 0.1944444444444444475, 0.2083333333333333426, 0.2222222222222222099, 0.2361111111111111049, 0.2500000000000000000, 0.2638888888888888951, 0.2777777777777777901, 0.2916666666666666852, 0.3055555555555555802, 0.3194444444444444198, 0.3333333333333333148, 0.3472222222222222099, 0.3611111111111111049, 0.3750000000000000000, 0.3888888888888888951, 0.4027777777777777901, 0.4166666666666666852, 0.4305555555555555802, 0.4444444444444444198, 0.4583333333333333148, 0.4722222222222222099, 0.4861111111111111049, 0.5000000000000000000, 0.5138888888888888395, 0.5277777777777777901, 0.5416666666666666297, 0.5555555555555555802, 0.5694444444444444198, 0.5833333333333333703, 0.5972222222222222099, 0.6111111111111111605, 0.6250000000000000000, 0.6388888888888888395, 0.6527777777777777901, 0.6666666666666666297, 0.6805555555555555802, 0.6944444444444444198, 0.7083333333333333703, 0.7222222222222222099, 0.7361111111111111605, 0.7500000000000000000, 0.7638888888888888395, 0.7777777777777777901, 0.7916666666666666297, 0.8055555555555555802, 0.8194444444444444198, 0.8333333333333333703, 0.8472222222222222099, 0.8611111111111111605, 0.8750000000000000000, 0.8888888888888888395, 0.9027777777777777901, 0.9166666666666666297, 0.9258785144422092550 ),
 .UNSPECIFIED. ) 
 GEOMETRIC_REPRESENTATION_ITEM ( )  RATIONAL_B_SPLINE_SURFACE ( (
 ( 1.000000000000000000, 0.8660254037844387076, 1.000000000000000000, 0.8660254037844387076, 1.000000000000000000, 0.8660254037844387076, 1.000000000000000000, 0.8660254037844387076, 1.000000000000000000, 0.8660254037844387076, 1.000000000000000000, 0.8660254037844387076, 1.000000000000000000, 0.8660254037844387076, 1.000000000000000000, 0.8660254037844387076, 1.000000000000000000, 0.8660254037844387076, 1.000000000000000000, 0.8660254037844387076, 1.000000000000000000, 0.8660254037844387076, 1.000000000000000000, 0.8660254037844387076, 1.000000000000000000, 0.8660254037844387076, 1.000000000000000000, 0.8660254037844387076, 1.000000000000000000, 0.8660254037844387076, 1.000000000000000000, 0.8660254037844387076, 1.000000000000000000, 0.8660254037844387076, 1.000000000000000000, 0.8660254037844387076, 1.000000000000000000, 0.8660254037844387076, 1.000000000000000000, 0.8660254037844387076, 1.000000000000000000, 0.8660254037844387076, 1.000000000000000000, 0.8660254037844387076, 1.000000000000000000, 0.8660254037844387076, 1.000000000000000000, 0.8660254037844387076, 1.000000000000000000, 0.8660254037844387076, 1.000000000000000000, 0.8660254037844387076, 1.000000000000000000, 0.8660254037844387076, 1.000000000000000000, 0.8660254037844387076, 1.000000000000000000, 0.8660254037844387076, 1.000000000000000000, 0.8660254037844387076, 1.000000000000000000, 0.8660254037844387076, 1.000000000000000000, 0.8660254037844387076, 1.000000000000000000, 0.8660254037844387076, 1.000000000000000000, 0.8660254037844387076, 1.000000000000000000, 0.8660254037844387076, 1.000000000000000000, 0.8660254037844387076, 1.000000000000000000, 0.8660254037844387076, 1.000000000000000000, 0.8660254037844387076, 1.000000000000000000, 0.8660254037844387076, 1.000000000000000000, 0.8660254037844387076, 1.000000000000000000, 0.8660254037844387076, 1.000000000000000000, 0.8660254037844387076, 1.000000000000000000, 0.8660254037844387076, 1.000000000000000000, 0.8660254037844387076, 1.000000000000000000, 0.8660254037844387076, 1.000000000000000000, 0.8660254037844387076, 1.000000000000000000, 0.8660254037844387076, 1.000000000000000000, 0.8660254037844387076, 1.000000000000000000, 0.8660254037844387076, 1.000000000000000000, 0.8660254037844387076, 1.000000000000000000, 0.8660254037844387076, 1.000000000000000000, 0.8660254037844387076, 1.000000000000000000, 0.8660254037844387076, 1.000000000000000000, 0.8660254037844387076, 1.000000000000000000, 0.8660254037844387076, 1.000000000000000000, 0.8660254037844387076, 1.000000000000000000, 0.8660254037844387076, 1.000000000000000000, 0.8660254037844387076, 1.000000000000000000, 0.8660254037844387076, 1.000000000000000000, 0.8660254037844387076, 1.000000000000000000, 0.8660254037844387076, 1.000000000000000000, 0.8660254037844387076, 1.000000000000000000, 0.8660254037844387076, 1.000000000000000000, 0.8660254037844387076, 1.000000000000000000, 0.8660254037844387076, 1.000000000000000000, 0.8660254037844387076, 1.000000000000000000, 0.9111409417988175496, 0.9401539645359766606),
 ( 1.000000000000000000, 0.8660254037844387076, 1.000000000000000000, 0.8660254037844387076, 1.000000000000000000, 0.8660254037844387076, 1.000000000000000000, 0.8660254037844387076, 1.000000000000000000, 0.8660254037844387076, 1.000000000000000000, 0.8660254037844387076, 1.000000000000000000, 0.8660254037844387076, 1.000000000000000000, 0.8660254037844387076, 1.000000000000000000, 0.8660254037844387076, 1.000000000000000000, 0.8660254037844387076, 1.000000000000000000, 0.8660254037844387076, 1.000000000000000000, 0.8660254037844387076, 1.000000000000000000, 0.8660254037844387076, 1.000000000000000000, 0.8660254037844387076, 1.000000000000000000, 0.8660254037844387076, 1.000000000000000000, 0.8660254037844387076, 1.000000000000000000, 0.8660254037844387076, 1.000000000000000000, 0.8660254037844387076, 1.000000000000000000, 0.8660254037844387076, 1.000000000000000000, 0.8660254037844387076, 1.000000000000000000, 0.8660254037844387076, 1.000000000000000000, 0.8660254037844387076, 1.000000000000000000, 0.8660254037844387076, 1.000000000000000000, 0.8660254037844387076, 1.000000000000000000, 0.8660254037844387076, 1.000000000000000000, 0.8660254037844387076, 1.000000000000000000, 0.8660254037844387076, 1.000000000000000000, 0.8660254037844387076, 1.000000000000000000, 0.8660254037844387076, 1.000000000000000000, 0.8660254037844387076, 1.000000000000000000, 0.8660254037844387076, 1.000000000000000000, 0.8660254037844387076, 1.000000000000000000, 0.8660254037844387076, 1.000000000000000000, 0.8660254037844387076, 1.000000000000000000, 0.8660254037844387076, 1.000000000000000000, 0.8660254037844387076, 1.000000000000000000, 0.8660254037844387076, 1.000000000000000000, 0.8660254037844387076, 1.000000000000000000, 0.8660254037844387076, 1.000000000000000000, 0.8660254037844387076, 1.000000000000000000, 0.8660254037844387076, 1.000000000000000000, 0.8660254037844387076, 1.000000000000000000, 0.8660254037844387076, 1.000000000000000000, 0.8660254037844387076, 1.000000000000000000, 0.8660254037844387076, 1.000000000000000000, 0.8660254037844387076, 1.000000000000000000, 0.8660254037844387076, 1.000000000000000000, 0.8660254037844387076, 1.000000000000000000, 0.8660254037844387076, 1.000000000000000000, 0.8660254037844387076, 1.000000000000000000, 0.8660254037844387076, 1.000000000000000000, 0.8660254037844387076, 1.000000000000000000, 0.8660254037844387076, 1.000000000000000000, 0.8660254037844387076, 1.000000000000000000, 0.8660254037844387076, 1.000000000000000000, 0.8660254037844387076, 1.000000000000000000, 0.8660254037844387076, 1.000000000000000000, 0.8660254037844387076, 1.000000000000000000, 0.8660254037844387076, 1.000000000000000000, 0.8660254037844387076, 1.000000000000000000, 0.8660254037844387076, 1.000000000000000000, 0.8660254037844387076, 1.000000000000000000, 0.8660254037844387076, 1.000000000000000000, 0.8660254037844387076, 1.000000000000000000, 0.8660254037844387076, 1.000000000000000000, 0.8660254037844387076, 1.000000000000000000, 0.9111409417988175496, 0.9401539645359766606) ) ) 
 REPRESENTATION_ITEM ( '' )  SURFACE ( )  );
#6613 = CARTESIAN_POINT ( 'NONE',  ( 79.39999999999999147, -32.92500000000000426, -99.99999999999998579 ) ) ;
#6614 = CARTESIAN_POINT ( 'NONE',  ( 83.60689295392862164, -35.00000000000000000, -97.24646917567282856 ) ) ;
#6615 = DIRECTION ( 'NONE',  ( -1.000000000000000000, 0.000000000000000000, -0.000000000000000000 ) ) ;
#6616 = EDGE_CURVE ( 'NONE', #11697, #3084, #2685, .T. ) ;
#6617 = CARTESIAN_POINT ( 'NONE',  ( 229.8435696437499871, -34.26562499938548001, 101.5914258081833879 ) ) ;
#6618 = CARTESIAN_POINT ( 'NONE',  ( -80.90000000000000568, -35.04768749875867684, 97.40192378864668399 ) ) ;
#6619 = ORIENTED_EDGE ( 'NONE', *, *, #16104, .T. ) ;
#6620 = CARTESIAN_POINT ( 'NONE',  ( 229.5999999999999375, -32.66249999999999432, 101.7320508075688821 ) ) ;
#6621 = CARTESIAN_POINT ( 'NONE',  ( 83.90000000000000568, -34.42500000000000426, -102.5980762113533018 ) ) ;
#6622 = CARTESIAN_POINT ( 'NONE',  ( -83.20384757729335945, -33.45134618820330985, -96.99999999999998579 ) ) ;
#6623 = DIRECTION ( 'NONE',  ( -1.000000000000000000, 0.000000000000000000, 0.000000000000000000 ) ) ;
#6624 = CARTESIAN_POINT ( 'NONE',  ( -82.40000000000000568, -34.55624999877097281, 97.00000000000000000 ) ) ;
#6625 = CARTESIAN_POINT ( 'NONE',  ( 79.64356964374999848, -30.47812499938548569, -99.99999999999998579 ) ) ;
#6626 = CARTESIAN_POINT ( 'NONE',  ( 81.59615242270665192, -34.81740381056767575, 97.00000000000000000 ) ) ;
#6627 = AXIS2_PLACEMENT_3D ( 'NONE', #10047, #12784, #1063 ) ;
#6628 = AXIS2_PLACEMENT_3D ( 'NONE', #35, #11937, #17908 ) ;
#6629 = ORIENTED_EDGE ( 'NONE', *, *, #12126, .F. ) ;
#6630 = CARTESIAN_POINT ( 'NONE',  ( 83.90000000000000568, -31.66874999877096997, 97.40192378864668399 ) ) ;
#6631 = SHAPE_DEFINITION_REPRESENTATION ( #15920, #4499 ) ;
#6632 = CARTESIAN_POINT ( 'NONE',  ( 232.5999999999999375, -33.29062499938547859, 103.1828516163667899 ) ) ;
#6633 = CARTESIAN_POINT ( 'NONE',  ( 231.2217848218749339, -33.47812499938547859, -52.38713871227520968 ) ) ;
#6634 = ADVANCED_FACE ( 'NONE', ( #5636 ), #15984, .F. ) ;
#6635 = CARTESIAN_POINT ( 'NONE',  ( -85.15643035624999868, -34.60312499938548569, 101.5914258081833879 ) ) ;
#6636 = CARTESIAN_POINT ( 'NONE',  ( 234.0999999999999375, -34.79999999999999716, -47.40192378864679768 ) ) ;
#6637 = VERTEX_POINT ( 'NONE', #14694 ) ;
#6638 = VERTEX_POINT ( 'NONE', #10024 ) ;
#6639 = CARTESIAN_POINT ( 'NONE',  ( -81.02178482187500208, -31.64062499938548356, -102.3871387122750889 ) ) ;
#6640 = EDGE_CURVE ( 'NONE', #138, #15818, #14760, .T. ) ;
#6641 = CARTESIAN_POINT ( 'NONE',  ( -83.90000000000000568, -32.17500000000000426, -97.40192378864668399 ) ) ;
#6642 = VERTEX_POINT ( 'NONE', #16747 ) ;
#6643 = CARTESIAN_POINT ( 'NONE',  ( 85.15643035625001289, -32.50312499938548427, 99.99999999999998579 ) ) ;
#6644 = CARTESIAN_POINT ( 'NONE',  ( -85.40000000000000568, -34.44374999877096855, -99.99999999999998579 ) ) ;
#6645 = CIRCLE ( 'NONE', #17560, 7.000000000000006217 ) ;
#6646 = CARTESIAN_POINT ( 'NONE',  ( 82.39999999999999147, -34.38750000000000284, 96.53589838486223584 ) ) ;
#6647 = VECTOR ( 'NONE', #8585, 1000.000000000000000 ) ;
#6648 = CARTESIAN_POINT ( 'NONE',  ( 100.0000000000000142, 20.19999999999999574, -140.0000000000000000 ) ) ;
#6649 = CARTESIAN_POINT ( 'NONE',  ( -80.90000000000000568, -30.99374999877096926, 97.40192378864668399 ) ) ;
#6650 = CARTESIAN_POINT ( 'NONE',  ( -85.40000000000000568, -34.40624999877096712, 101.7320508075688679 ) ) ;
#6651 = FACE_OUTER_BOUND ( 'NONE', #2111, .T. ) ;
#6652 = CARTESIAN_POINT ( 'NONE',  ( 79.39999999999999147, -34.21874999877096712, -99.99999999999998579 ) ) ;
#6653 = EDGE_CURVE ( 'NONE', #6130, #9315, #3410, .T. ) ;
#6654 = CARTESIAN_POINT ( 'NONE',  ( 85.40000000000000568, -30.39374999877097139, -99.99999999999998579 ) ) ;
#6655 = CARTESIAN_POINT ( 'NONE',  ( 231.2217848218749339, -32.91562499938547148, 97.61286128772489690 ) ) ;
#6656 = ORIENTED_EDGE ( 'NONE', *, *, #3609, .T. ) ;
#6657 = CARTESIAN_POINT ( 'NONE',  ( 79.64356964374998427, -33.55312499938548854, -101.5914258081833879 ) ) ;
#6658 = CARTESIAN_POINT ( 'NONE',  ( -85.15643035625001289, -35.09062499938548285, -99.99999999999998579 ) ) ;
#6659 = DIRECTION ( 'NONE',  ( 1.000000000000000000, -1.387778780781445676E-15, -2.407412430484046130E-31 ) ) ;
#6660 = CIRCLE ( 'NONE', #1039, 7.500000000000020428 ) ;
#6661 = VERTEX_POINT ( 'NONE', #6305 ) ;
#6662 = CARTESIAN_POINT ( 'NONE',  ( -82.40000000000000568, -50.00000000000000000, 99.99999999999998579 ) ) ;
#6663 = DIRECTION ( 'NONE',  ( 0.000000000000000000, -0.000000000000000000, -1.000000000000000000 ) ) ;
#6664 = CARTESIAN_POINT ( 'NONE',  ( 105.1999999999999886, -4.999999999999993783, -103.0000000000000995 ) ) ;
#6665 = ORIENTED_EDGE ( 'NONE', *, *, #3294, .T. ) ;
#6666 = DIRECTION ( 'NONE',  ( -1.000000000000000000, 0.000000000000000000, 0.000000000000000000 ) ) ;
#6667 = CARTESIAN_POINT ( 'NONE',  ( 4.000000000000000000, -2.309401076758514915, -3.433295621305383349 ) ) ;
#6668 = EDGE_LOOP ( 'NONE', ( #8943, #6495 ) ) ;
#6669 =( BOUNDED_CURVE ( )  B_SPLINE_CURVE ( 2, ( #3521, #9578, #2159, #12320, #17006, #5005, #8012, #15151, #18576 ),
 .UNSPECIFIED., .F., .F. ) 
 B_SPLINE_CURVE_WITH_KNOTS ( ( 3, 2, 2, 2, 3 ),
 ( 0.3125000000000000555, 0.3194444444444444198, 0.3333333333333333148, 0.3472222222222222099, 0.3541666666666666852 ),
 .UNSPECIFIED. ) 
 CURVE ( )  GEOMETRIC_REPRESENTATION_ITEM ( )  RATIONAL_B_SPLINE_CURVE ( ( 0.9330127018922192983, 0.9330127018922198534, 1.000000000000000000, 0.8660254037844387076, 1.000000000000000000, 0.8660254037844387076, 1.000000000000000000, 0.9330127018922190762, 0.9330127018922194093 ) ) 
 REPRESENTATION_ITEM ( '' )  );
#6670 = SURFACE_STYLE_FILL_AREA ( #3724 ) ;
#6671 = CARTESIAN_POINT ( 'NONE',  ( 85.40000000000000568, -30.41249999999999787, -101.7320508075688679 ) ) ;
#6672 = EDGE_CURVE ( 'NONE', #18169, #13093, #4268, .T. ) ;
#6673 = CARTESIAN_POINT ( 'NONE',  ( -79.64356964374999848, -34.98839802032724577, -99.56403331587389971 ) ) ;
#6674 = B_SPLINE_CURVE_WITH_KNOTS ( 'NONE', 3,
 ( #4232, #2764, #10382, #7450, #15065, #13409, #2954, #11941, #18826, #5448, #14870, #11386, #4331, #8720, #14673, #39 ),
 .UNSPECIFIED., .F., .F.,
 ( 4, 2, 2, 2, 2, 2, 2, 4 ),
 ( 0.000000000000000000, 0.0005391024520904326520, 0.001078204904180865304, 0.002156409808361677265, 0.002695512260452082812, 0.003234614712542487492, 0.003773717164632892172, 0.004312819616723297285 ),
 .UNSPECIFIED. ) ;
#6675 = CARTESIAN_POINT ( 'NONE',  ( -82.39999999999999147, -34.33124999877097139, 103.4641016151377499 ) ) ;
#6676 = CARTESIAN_POINT ( 'NONE',  ( -82.39999999999999147, -30.33750000000000213, 103.4641016151377499 ) ) ;
#6677 = CARTESIAN_POINT ( 'NONE',  ( 232.3466685930879123, -34.99995246259152282, -52.98928446312130802 ) ) ;
#6678 = LINE ( 'NONE', #6575, #5085 ) ;
#6679 = DIRECTION ( 'NONE',  ( 0.000000000000000000, 0.000000000000000000, 1.000000000000000000 ) ) ;
#6680 = CARTESIAN_POINT ( 'NONE',  ( -82.39999999999999147, -33.85312499938547859, 96.81714838363319586 ) ) ;
#6681 = PLANE ( 'NONE',  #5232 ) ;
#6682 = EDGE_LOOP ( 'NONE', ( #689, #9486, #1819, #16263 ) ) ;
#6683 = CARTESIAN_POINT ( 'NONE',  ( 229.5999999999999375, -34.49999999999999289, -50.00000000000011369 ) ) ;
#6684 = CARTESIAN_POINT ( 'NONE',  ( -85.40000000000000568, -34.05000000000000426, 99.99999999999998579 ) ) ;
#6685 = CARTESIAN_POINT ( 'NONE',  ( -83.90000000000000568, -34.06874999877096855, 97.40192378864668399 ) ) ;
#6686 = CARTESIAN_POINT ( 'NONE',  ( 83.20384757729335945, -33.69240381056766154, 102.9999999999999858 ) ) ;
#6687 = CARTESIAN_POINT ( 'NONE',  ( -85.15643035624999868, -34.79062499938548569, 98.40857419181659793 ) ) ;
#6688 = CARTESIAN_POINT ( 'NONE',  ( 232.5999999999999375, -31.37812499938547717, -46.81714838363331666 ) ) ;
#6689 = CARTESIAN_POINT ( 'NONE',  ( -79.39999999999999147, -32.92500000000000426, 99.99999999999998579 ) ) ;
#6690 = ORIENTED_EDGE ( 'NONE', *, *, #2648, .F. ) ;
#6691 = CARTESIAN_POINT ( 'NONE',  ( 0.3126073911696399255, 2.020725942163686728, -3.499999999999999556 ) ) ;
#6692 = CARTESIAN_POINT ( 'NONE',  ( -82.40000000000000568, -33.71249999999998437, -102.9999999999999858 ) ) ;
#6693 = CARTESIAN_POINT ( 'NONE',  ( 83.77821517812500929, -32.01562499938548001, 102.3871387122750889 ) ) ;
#6694 = CARTESIAN_POINT ( 'NONE',  ( 84.82992844608112648, -31.99999999999999289, -98.68659295968670619 ) ) ;
#6695 =( BOUNDED_CURVE ( )  B_SPLINE_CURVE ( 2, ( #1638, #16873, #7878, #6329, #16585, #12085, #10619, #4670, #9147 ),
 .UNSPECIFIED., .F., .F. ) 
 B_SPLINE_CURVE_WITH_KNOTS ( ( 3, 2, 2, 2, 3 ),
 ( 0.8125000000000001110, 0.8194444444444444198, 0.8333333333333333703, 0.8472222222222222099, 0.8530683953269213582 ),
 .UNSPECIFIED. ) 
 CURVE ( )  GEOMETRIC_REPRESENTATION_ITEM ( )  RATIONAL_B_SPLINE_CURVE ( ( 0.9330127018922194093, 0.9330127018922204085, 1.000000000000000000, 0.8660254037844387076, 1.000000000000000000, 0.8660254037844387076, 1.000000000000000000, 0.9436068149601996025, 0.9346881722405915305 ) ) 
 REPRESENTATION_ITEM ( '' )  );
#6696 = CARTESIAN_POINT ( 'NONE',  ( -81.02178482187500208, -33.10312499938548569, 97.61286128772489690 ) ) ;
#6697 = LINE ( 'NONE', #4845, #9545 ) ;
#6698 = CARTESIAN_POINT ( 'NONE',  ( 81.02178482187500208, -31.34062499938548996, 97.61286128772489690 ) ) ;
#6699 = CARTESIAN_POINT ( 'NONE',  ( 79.64356964375001269, -32.31562499938548427, -101.5914258081833879 ) ) ;
#6700 = CARTESIAN_POINT ( 'NONE',  ( 233.9782151781249411, -32.09062499938547575, -52.38713871227520968 ) ) ;
#6701 = CARTESIAN_POINT ( 'NONE',  ( -79.64356964374998427, -34.49062499938548854, 98.40857419181659793 ) ) ;
#6702 = CARTESIAN_POINT ( 'NONE',  ( -85.15643035625001289, -31.49062499938548498, -99.99999999999998579 ) ) ;
#6703 = EDGE_LOOP ( 'NONE', ( #7340, #16297, #6274, #7420 ) ) ;
#6704 = CARTESIAN_POINT ( 'NONE',  ( 85.15643035625001289, -32.05312499938548854, 99.99999999999998579 ) ) ;
#6705 = CARTESIAN_POINT ( 'NONE',  ( -85.40000000000000568, -33.05624999877097281, 101.7320508075688821 ) ) ;
#6706 = CARTESIAN_POINT ( 'NONE',  ( -85.15643035625001289, -30.59062499938548285, 99.99999999999998579 ) ) ;
#6707 = CARTESIAN_POINT ( 'NONE',  ( -81.02178482187500208, -34.90312499938548285, 97.61286128772489690 ) ) ;
#6708 = CARTESIAN_POINT ( 'NONE',  ( -82.39999999999999147, -31.46249999999999858, 96.99999999999998579 ) ) ;
#6709 = VERTEX_POINT ( 'NONE', #16465 ) ;
#6710 = CARTESIAN_POINT ( 'NONE',  ( -80.90000000000000568, -32.40000000000000568, -102.5980762113533018 ) ) ;
#6711 = DIRECTION ( 'NONE',  ( -4.415659757031858318E-14, 1.577021341797092166E-14, 1.000000000000000000 ) ) ;
#6712 = CARTESIAN_POINT ( 'NONE',  ( 5.599999999999999645, 4.041451884327382338, 2.749426538070117193E-16 ) ) ;
#6713 = CARTESIAN_POINT ( 'NONE',  ( -81.59615242270662350, -32.96115380933864003, 103.0000000000000000 ) ) ;
#6714 = CARTESIAN_POINT ( 'NONE',  ( 229.8435696437499871, -31.07812499938548001, 98.40857419181659793 ) ) ;
#6715 = CARTESIAN_POINT ( 'NONE',  ( -82.39999999999999147, -33.21018749875868536, 96.53589838486223584 ) ) ;
#6716 = CARTESIAN_POINT ( 'NONE',  ( 3.383466608491643077E-15, 4.736522675502341073, -3.681124513963742739 ) ) ;
#6717 = CARTESIAN_POINT ( 'NONE',  ( 232.5999999999999091, -33.03749999999998721, 102.9999999999999858 ) ) ;
#6718 = CARTESIAN_POINT ( 'NONE',  ( 82.39999999999999147, -34.75312499938548427, 103.1828516163667899 ) ) ;
#6719 = CARTESIAN_POINT ( 'NONE',  ( 85.15643035625001289, -31.15312499938548996, 99.99999999999998579 ) ) ;
#6720 = CARTESIAN_POINT ( 'NONE',  ( 249.9999999999999716, -35.00000000000000000, -100.0000000000000000 ) ) ;
#6721 = CARTESIAN_POINT ( 'NONE',  ( 229.5999999999999375, -34.93124999877095860, -51.73205080756898866 ) ) ;
#6722 = CARTESIAN_POINT ( 'NONE',  ( 83.77821517812500929, -31.97812499938548925, -102.3871387122750889 ) ) ;
#6723 = CARTESIAN_POINT ( 'NONE',  ( 229.5999999999999659, -34.97364041986482874, 98.90809577818232867 ) ) ;
#6724 = ADVANCED_FACE ( 'NONE', ( #6111 ), #12061, .F. ) ;
#6725 = VERTEX_POINT ( 'NONE', #3841 ) ;
#6726 = CARTESIAN_POINT ( 'NONE',  ( 232.5999999999999943, -34.86562499938548143, -53.18285161636690361 ) ) ;
#6727 = CARTESIAN_POINT ( 'NONE',  ( 233.9782151781249411, -32.20312499938548001, 97.61286128772489690 ) ) ;
#6728 = CARTESIAN_POINT ( 'NONE',  ( 231.2217848218749339, -31.97812499938548214, -47.61286128772501769 ) ) ;
#6729 = ADVANCED_FACE ( 'NONE', ( #5226 ), #18709, .T. ) ;
#6730 =( BOUNDED_CURVE ( )  B_SPLINE_CURVE ( 3, ( #11007, #3586, #9546, #3876 ),
 .UNSPECIFIED., .F., .F. ) 
 B_SPLINE_CURVE_WITH_KNOTS ( ( 4, 4 ),
 ( 4.712388980384689674, 6.283185307179586232 ),
 .UNSPECIFIED. ) 
 CURVE ( )  GEOMETRIC_REPRESENTATION_ITEM ( )  RATIONAL_B_SPLINE_CURVE ( ( 1.000000000000000000, 0.8047378541243649375, 0.8047378541243649375, 1.000000000000000000 ) ) 
 REPRESENTATION_ITEM ( '' )  );
#6731 = EDGE_CURVE ( 'NONE', #7323, #10655, #17641, .T. ) ;
#6732 = CARTESIAN_POINT ( 'NONE',  ( -85.15643035625001289, -33.29062499938547859, 99.99999999999998579 ) ) ;
#6733 = DIRECTION ( 'NONE',  ( -0.000000000000000000, -1.000000000000000000, -0.000000000000000000 ) ) ;
#6734 = ORIENTED_EDGE ( 'NONE', *, *, #13692, .F. ) ;
#6735 = VERTEX_POINT ( 'NONE', #9807 ) ;
#6736 = CARTESIAN_POINT ( 'NONE',  ( -85.15643035624999868, -32.42812499938548854, -101.5914258081833879 ) ) ;
#6737 = CYLINDRICAL_SURFACE ( 'NONE', #4748, 3.000000000000009770 ) ;
#6738 = ORIENTED_EDGE ( 'NONE', *, *, #2354, .T. ) ;
#6739 = CARTESIAN_POINT ( 'NONE',  ( 83.77821517812500929, -33.77812499938548285, 97.61286128772489690 ) ) ;
#6740 = CARTESIAN_POINT ( 'NONE',  ( -82.39999999999999147, -34.55624999877096570, -103.4641016151377499 ) ) ;
#6741 = DIRECTION ( 'NONE',  ( 0.000000000000000000, 0.000000000000000000, 1.000000000000000000 ) ) ;
#6742 = CARTESIAN_POINT ( 'NONE',  ( -80.03686793005704203, -35.00000000000000000, 98.35371953419887348 ) ) ;
#6743 = CARTESIAN_POINT ( 'NONE',  ( -85.40000000000000568, -33.13124999877096855, 98.26794919243111792 ) ) ;
#6744 = CARTESIAN_POINT ( 'NONE',  ( -80.90000000000000568, -34.59374999877096712, 97.40192378864668399 ) ) ;
#6745 = CARTESIAN_POINT ( 'NONE',  ( 244.7999999999999545, -32.00000000000000711, -97.80000000000002558 ) ) ;
#6746 = EDGE_CURVE ( 'NONE', #15232, #11798, #16759, .T. ) ;
#6747 = B_SPLINE_CURVE_WITH_KNOTS ( 'NONE', 3,
 ( #7626, #17799, #13291, #16332, #11833, #10653, #13580, #11927, #6174, #6077, #2941, #16527, #14957, #16620, #4410, #3128, #10367, #7529 ),
 .UNSPECIFIED., .F., .F.,
 ( 4, 2, 2, 2, 2, 2, 2, 2, 4 ),
 ( 0.000000000000000000, 0.0007106627595358627324, 0.001421325519071725465, 0.002131988278607587980, 0.002842651038143450930, 0.003553313797679313879, 0.004263976557215175961, 0.004974639316751038910, 0.005685302076286901860 ),
 .UNSPECIFIED. ) ;
#6748 = CARTESIAN_POINT ( 'NONE',  ( 111.0000000000000000, 10.19999999999997620, -142.6499999999999773 ) ) ;
#6749 = ADVANCED_FACE ( 'NONE', ( #6794 ), #13810, .F. ) ;
#6750 = CARTESIAN_POINT ( 'NONE',  ( 233.5451393107506135, -32.00000000000000711, 102.7533691519571164 ) ) ;
#6751 = CARTESIAN_POINT ( 'NONE',  ( 235.3564303562499447, -34.37812499938547717, 98.40857419181659793 ) ) ;
#6752 = EDGE_CURVE ( 'NONE', #7637, #2550, #1418, .T. ) ;
#6753 = VERTEX_POINT ( 'NONE', #12446 ) ;
#6754 = CARTESIAN_POINT ( 'NONE',  ( 79.64356964374998427, -33.47812499938547859, -98.40857419181659793 ) ) ;
#6755 =( NAMED_UNIT ( * ) PLANE_ANGLE_UNIT ( ) SI_UNIT ( $, .RADIAN. ) );
#6756 = CARTESIAN_POINT ( 'NONE',  ( 235.5999999999999375, -31.51874999877096073, 99.99999999999998579 ) ) ;
#6757 = DIRECTION ( 'NONE',  ( 0.000000000000000000, -1.000000000000000000, 0.000000000000000000 ) ) ;
#6758 = ORIENTED_EDGE ( 'NONE', *, *, #4863, .T. ) ;
#6759 = CIRCLE ( 'NONE', #17982, 2.500000000000000444 ) ;
#6760 = CARTESIAN_POINT ( 'NONE',  ( 229.5999999999999375, -32.60624999877096286, 101.7320508075688821 ) ) ;
#6761 = CARTESIAN_POINT ( 'NONE',  ( -81.02178482187500208, -31.19062499938548427, 97.61286128772489690 ) ) ;
#6762 = LINE ( 'NONE', #15839, #4765 ) ;
#6763 = ORIENTED_EDGE ( 'NONE', *, *, #11143, .T. ) ;
#6764 = CARTESIAN_POINT ( 'NONE',  ( 4.033901012036456457, -3.740908793663545673, 0.5205559028932933430 ) ) ;
#6765 = DIRECTION ( 'NONE',  ( 4.625929269271485174E-17, 1.000000000000000000, -0.000000000000000000 ) ) ;
#6766 = ORIENTED_EDGE ( 'NONE', *, *, #12697, .T. ) ;
#6767 = CARTESIAN_POINT ( 'NONE',  ( 249.9999999999999716, -29.80000000000000426, -100.0000000000000000 ) ) ;
#6768 = CARTESIAN_POINT ( 'NONE',  ( 79.39999999999999147, -33.86250000000000426, -101.7320508075688537 ) ) ;
#6769 = CYLINDRICAL_SURFACE ( 'NONE', #3309, 3.000000000000002665 ) ;
#6770 = AXIS2_PLACEMENT_3D ( 'NONE', #15317, #106, #14939 ) ;
#6771 = CARTESIAN_POINT ( 'NONE',  ( -82.39999999999999147, -33.88124999877096855, 103.4641016151377499 ) ) ;
#6772 = CARTESIAN_POINT ( 'NONE',  ( -79.39999999999999147, -34.30856250001229313, 101.7320508075688537 ) ) ;
#6773 = CARTESIAN_POINT ( 'NONE',  ( -82.39999999999999147, -33.20624999877097849, 97.00000000000000000 ) ) ;
#6774 = CARTESIAN_POINT ( 'NONE',  ( 80.90000000000000568, -33.24374999877097281, 102.5980762113533018 ) ) ;
#6775 = CARTESIAN_POINT ( 'NONE',  ( 82.40000000000001990, -33.88124999877096855, 97.00000000000000000 ) ) ;
#6776 = DIRECTION ( 'NONE',  ( 0.000000000000000000, -1.000000000000000000, 0.000000000000000000 ) ) ;
#6777 = CARTESIAN_POINT ( 'NONE',  ( -83.77821517812500929, -32.76562499938548711, 102.3871387122750889 ) ) ;
#6778 = CYLINDRICAL_SURFACE ( 'NONE', #10522, 3.000000000000002665 ) ;
#6779 = ORIENTED_EDGE ( 'NONE', *, *, #14731, .T. ) ;
#6780 = B_SPLINE_CURVE_WITH_KNOTS ( 'NONE', 3,
 ( #12634, #5328, #12538, #5225, #12834, #6691 ),
 .UNSPECIFIED., .F., .F.,
 ( 4, 2, 4 ),
 ( 0.002044882221487534513, 0.003063384235218497183, 0.004081886248949459853 ),
 .UNSPECIFIED. ) ;
#6781 = CARTESIAN_POINT ( 'NONE',  ( 235.5999999999999943, -34.68749999999999289, -51.73205080756900287 ) ) ;
#6782 = ADVANCED_FACE ( 'NONE', ( #451 ), #11073, .T. ) ;
#6783 = CARTESIAN_POINT ( 'NONE',  ( 234.0999999999999375, -33.24374999877096570, -52.59807621135342970 ) ) ;
#6784 = B_SPLINE_CURVE_WITH_KNOTS ( 'NONE', 3,
 ( #13527, #1710, #7665, #10506, #19316, #13721, #17754, #13621, #14903, #16473, #3078, #9038, #15003, #2889, #8845, #165, #16752, #11181 ),
 .UNSPECIFIED., .F., .F.,
 ( 4, 2, 2, 2, 2, 2, 2, 2, 4 ),
 ( 0.000000000000000000, 0.0007089252359871075744, 0.001417850471974215149, 0.002126775707961322832, 0.002835700943948430298, 0.003544626179935537764, 0.004253551415922645663, 0.004962476651909753129, 0.005671401887896860596 ),
 .UNSPECIFIED. ) ;
#6785 = DIRECTION ( 'NONE',  ( -1.000000000000000000, 0.000000000000000000, 0.000000000000000000 ) ) ;
#6786 = CARTESIAN_POINT ( 'NONE',  ( 233.9782151781249411, -32.65312499938548285, 97.61286128772489690 ) ) ;
#6787 = CARTESIAN_POINT ( 'NONE',  ( -79.64356964375001269, -33.59062499938548285, 98.40857419181659793 ) ) ;
#6788 = CARTESIAN_POINT ( 'NONE',  ( 235.3564303562499447, -30.32812499938548001, -51.59142580818350865 ) ) ;
#6789 = CIRCLE ( 'NONE', #13675, 5.371010071662833063 ) ;
#6790 = ORIENTED_EDGE ( 'NONE', *, *, #11964, .F. ) ;
#6791 = DIRECTION ( 'NONE',  ( -0.000000000000000000, 1.000000000000000000, -0.000000000000000000 ) ) ;
#6792 = EDGE_CURVE ( 'NONE', #14066, #1594, #11827, .T. ) ;
#6793 =( BOUNDED_SURFACE ( )  B_SPLINE_SURFACE ( 3, 2, ( 
 ( #308, #6064, #5966 ),
 ( #4690, #6161, #15136 ),
 ( #16321, #11914, #17887 ),
 ( #13279, #10640, #14946 ),
 ( #17983, #10449, #16607 ),
 ( #16513, #17791, #16229 ) ),
 .UNSPECIFIED., .F., .F., .F. ) 
 B_SPLINE_SURFACE_WITH_KNOTS ( ( 4, 2, 4 ),
 ( 3, 3 ),
 ( 0.02027752710269158445, 0.02273781595091097299, 0.02519810479913036153 ),
 ( 0.000000000000000000, 1.000000000000000000 ),
 .UNSPECIFIED. ) 
 GEOMETRIC_REPRESENTATION_ITEM ( )  RATIONAL_B_SPLINE_SURFACE ( (
 ( 1.000000000000000000, 0.8047781431712808242, 1.000000000000000000),
 ( 1.000000000000000000, 0.8123773247083928561, 1.000000000000000000),
 ( 1.000000000000000000, 0.8190670192154906326, 1.000000000000000000),
 ( 1.000000000000000000, 0.8192353552912178261, 1.000000000000000000),
 ( 1.000000000000000000, 0.8126132098226825917, 1.000000000000000000),
 ( 1.000000000000000000, 0.8047712465856394770, 1.000000000000000000) ) ) 
 REPRESENTATION_ITEM ( '' )  SURFACE ( )  );
#6794 = FACE_OUTER_BOUND ( 'NONE', #2629, .T. ) ;
#6795 = CARTESIAN_POINT ( 'NONE',  ( 83.77821517812500929, -32.76562499938548711, 97.61286128772489690 ) ) ;
#6796 = AXIS2_PLACEMENT_3D ( 'NONE', #1770, #7730, #6279 ) ;
#6797 = CARTESIAN_POINT ( 'NONE',  ( 231.0999999999999375, -33.01874999877096428, -47.40192378864679768 ) ) ;
#6798 = CARTESIAN_POINT ( 'NONE',  ( 229.8435696437499587, -32.42812499938548143, -51.59142580818350154 ) ) ;
#6799 = CARTESIAN_POINT ( 'NONE',  ( -79.64356964374999848, -33.17812499938548854, 99.99999999999998579 ) ) ;
#6800 = CARTESIAN_POINT ( 'NONE',  ( -79.64356964374998427, -34.11562499938548854, -98.40857419181659793 ) ) ;
#6801 = CARTESIAN_POINT ( 'NONE',  ( 85.15643035624999868, -31.52812499938547930, 101.5914258081833879 ) ) ;
#6802 = COLOUR_RGB ( '',0.8941176470588234615, 0.8941176470588234615, 0.8941176470588234615 ) ;
#6803 = CARTESIAN_POINT ( 'NONE',  ( 85.15643035625001289, -34.30312499938548854, -99.99999999999998579 ) ) ;
#6804 = CARTESIAN_POINT ( 'NONE',  ( 231.2217848218749339, -33.21562499938547575, -47.61286128772501769 ) ) ;
#6805 = CARTESIAN_POINT ( 'NONE',  ( -81.02178482187500208, -34.49062499938548854, 102.3871387122750889 ) ) ;
#6806 = EDGE_LOOP ( 'NONE', ( #6942, #13539, #7564, #7804 ) ) ;
#6807 = CARTESIAN_POINT ( 'NONE',  ( 85.15643035625001289, -31.60312499938548569, 99.99999999999998579 ) ) ;
#6808 = VECTOR ( 'NONE', #7057, 1000.000000000000000 ) ;
#6809 = CARTESIAN_POINT ( 'NONE',  ( -83.90000000000000568, -32.32500000000000284, 97.40192378864668399 ) ) ;
#6810 = CARTESIAN_POINT ( 'NONE',  ( -79.64356964375001269, -30.85312499938548569, 101.5914258081833879 ) ) ;
#6811 = CARTESIAN_POINT ( 'NONE',  ( -79.64356964375001269, -31.67812499938548143, 98.40857419181659793 ) ) ;
#6812 = CARTESIAN_POINT ( 'NONE',  ( -94.79999999999999716, -32.00000000000000000, 150.0000000000000000 ) ) ;
#6813 = EDGE_LOOP ( 'NONE', ( #3333, #19226, #3177 ) ) ;
#6814 = CARTESIAN_POINT ( 'NONE',  ( -85.40000000000000568, -34.50000000000000000, -99.99999999999998579 ) ) ;
#6815 = AXIS2_PLACEMENT_3D ( 'NONE', #18017, #9106, #16730 ) ;
#6816 = FACE_OUTER_BOUND ( 'NONE', #12301, .T. ) ;
#6817 = CARTESIAN_POINT ( 'NONE',  ( -85.40000000000000568, -30.00000000000000355, 99.99999999999998579 ) ) ;
#6818 = CARTESIAN_POINT ( 'NONE',  ( -82.40000000000000568, -30.00000000000000355, 99.99999999999998579 ) ) ;
#6819 = CARTESIAN_POINT ( 'NONE',  ( -83.20384757729338787, -34.59240381056766722, 97.00000000000000000 ) ) ;
#6820 = VECTOR ( 'NONE', #7016, 1000.000000000000000 ) ;
#6821 = CARTESIAN_POINT ( 'NONE',  ( -82.85024983566745505, -35.00000000000000711, 97.02690897175904183 ) ) ;
#6822 = FACE_OUTER_BOUND ( 'NONE', #18291, .T. ) ;
#6823 = CARTESIAN_POINT ( 'NONE',  ( 81.02178482187500208, -34.94062499938548427, 97.61286128772489690 ) ) ;
#6824 = CARTESIAN_POINT ( 'NONE',  ( 83.77821517812500929, -31.07812499938548711, 97.61286128772489690 ) ) ;
#6825 = DIRECTION ( 'NONE',  ( 1.000000000000000000, 0.000000000000000000, 0.000000000000000000 ) ) ;
#6826 = EDGE_CURVE ( 'NONE', #5168, #14858, #6277, .T. ) ;
#6827 = CARTESIAN_POINT ( 'NONE',  ( -83.90000000000000568, -32.77499999999999858, -102.5980762113533018 ) ) ;
#6828 = CARTESIAN_POINT ( 'NONE',  ( 79.64356964375001269, -31.79062499938548569, -98.40857419181659793 ) ) ;
#6829 = AXIS2_PLACEMENT_3D ( 'NONE', #3875, #11399, #14507 ) ;
#6830 = CARTESIAN_POINT ( 'NONE',  ( 4.165266963751923512, 2.049631966911918735, 3.550066703508774957 ) ) ;
#6831 = ORIENTED_EDGE ( 'NONE', *, *, #4115, .T. ) ;
#6832 = CARTESIAN_POINT ( 'NONE',  ( 229.8435696437499587, -34.71562499938547575, -48.40857419181671162 ) ) ;
#6833 = PRODUCT_CONTEXT ( 'NONE', #4969, 'mechanical' ) ;
#6834 = CARTESIAN_POINT ( 'NONE',  ( 233.7151113960924818, -35.00000000000002842, -47.47285052570518360 ) ) ;
#6835 = CARTESIAN_POINT ( 'NONE',  ( 231.2217848218749339, -33.02812499938547575, -52.38713871227520968 ) ) ;
#6836 = CARTESIAN_POINT ( 'NONE',  ( -83.77821517812500929, -33.21562499938548285, 102.3871387122750889 ) ) ;
#6837 = CARTESIAN_POINT ( 'NONE',  ( 4.630153689607048761, 0.000000000000000000, -5.371010071662833063 ) ) ;
#6838 = ORIENTED_EDGE ( 'NONE', *, *, #19299, .T. ) ;
#6839 = CARTESIAN_POINT ( 'NONE',  ( -79.64356964375001269, -31.67812499938548143, -101.5914258081833879 ) ) ;
#6840 = CYLINDRICAL_SURFACE ( 'NONE', #11291, 3.000000000000002665 ) ;
#6841 = EDGE_LOOP ( 'NONE', ( #3699, #13865, #14193, #2144 ) ) ;
#6842 = CARTESIAN_POINT ( 'NONE',  ( 79.64356964374998427, -34.49062499938548854, 101.5914258081833879 ) ) ;
#6843 = CARTESIAN_POINT ( 'NONE',  ( -85.15643035624999868, -31.64062499938548356, -101.5914258081833879 ) ) ;
#6844 = DIRECTION ( 'NONE',  ( 1.000000000000000000, 0.000000000000000000, -0.000000000000000000 ) ) ;
#6845 = CARTESIAN_POINT ( 'NONE',  ( -83.90000000000000568, -32.11874999877097281, 102.5980762113533018 ) ) ;
#6846 = CARTESIAN_POINT ( 'NONE',  ( -82.39999999999999147, -31.49062499938548854, 103.1828516163667899 ) ) ;
#6847 = CARTESIAN_POINT ( 'NONE',  ( -81.02178482187500208, -33.59062499938548285, -97.61286128772489690 ) ) ;
#6848 = EDGE_CURVE ( 'NONE', #12516, #4275, #15870, .T. ) ;
#6849 = CARTESIAN_POINT ( 'NONE',  ( 234.4730806518346924, -35.00000000000001421, 102.0537355158135568 ) ) ;
#6850 = CARTESIAN_POINT ( 'NONE',  ( 231.9083760470965103, -32.00000000000000711, 102.7516965079134081 ) ) ;
#6851 = CARTESIAN_POINT ( 'NONE',  ( 229.5999999999999375, -30.41249999999999076, 101.7320508075688679 ) ) ;
#6852 = VERTEX_POINT ( 'NONE', #930 ) ;
#6853 = CARTESIAN_POINT ( 'NONE',  ( 79.64356964374998427, -32.65312499938548285, -101.5914258081833879 ) ) ;
#6854 = CARTESIAN_POINT ( 'NONE',  ( 234.0999999999999375, -30.99374999877096215, 97.40192378864668399 ) ) ;
#6855 = CARTESIAN_POINT ( 'NONE',  ( 231.0999999999999375, -32.11874999877096570, -47.40192378864679768 ) ) ;
#6856 = ORIENTED_EDGE ( 'NONE', *, *, #11503, .T. ) ;
#6857 = B_SPLINE_CURVE_WITH_KNOTS ( 'NONE', 3,
 ( #9044, #13725, #366, #15007, #15100, #2893, #1431, #10510, #3271, #9227, #1809, #9135, #268, #18048, #8941, #4458 ),
 .UNSPECIFIED., .F., .F.,
 ( 4, 2, 2, 2, 2, 2, 2, 4 ),
 ( 0.000000000000000000, 0.0005391024520904310257, 0.001078204904180862051, 0.002156409808361698516, 0.002695512260452095389, 0.003234614712542491395, 0.003773717164632888268, 0.004312819616723284274 ),
 .UNSPECIFIED. ) ;
#6858 = CARTESIAN_POINT ( 'NONE',  ( -82.39999999999999147, -33.65624999877097423, 97.00000000000000000 ) ) ;
#6859 = CARTESIAN_POINT ( 'NONE',  ( -83.77821517812500929, -30.96562499938548640, 102.3871387122750889 ) ) ;
#6860 = FACE_OUTER_BOUND ( 'NONE', #10242, .T. ) ;
#6861 = ORIENTED_EDGE ( 'NONE', *, *, #12119, .T. ) ;
#6862 = CARTESIAN_POINT ( 'NONE',  ( 3.878096787214261987, -2.680238624821020377, 2.357690525401458181 ) ) ;
#6864 = EDGE_CURVE ( 'NONE', #9562, #2447, #3895, .T. ) ;
#6863 = CARTESIAN_POINT ( 'NONE',  ( 4.170895651974601215, -2.054890354522714180, 3.559174498016426824 ) ) ;
#6865 = VERTEX_POINT ( 'NONE', #14675 ) ;
#6866 = CARTESIAN_POINT ( 'NONE',  ( 79.39999999999999147, -32.92500000000000426, -99.99999999999998579 ) ) ;
#6867 = FACE_OUTER_BOUND ( 'NONE', #6541, .T. ) ;
#6868 = CARTESIAN_POINT ( 'NONE',  ( -79.64356964374999848, -30.47812499938548569, 99.99999999999998579 ) ) ;
#6869 = CARTESIAN_POINT ( 'NONE',  ( -83.90000000000000568, -33.67106250001229739, 97.40192378864668399 ) ) ;
#6870 = CARTESIAN_POINT ( 'NONE',  ( 233.4038475772933623, -32.32634618820329564, -53.00000000000011369 ) ) ;
#6871 = CARTESIAN_POINT ( 'NONE',  ( 233.7735609739809490, -31.99999999999998579, -52.66365949829813786 ) ) ;
#6872 = EDGE_CURVE ( 'NONE', #15407, #1665, #17620, .T. ) ;
#6873 = CARTESIAN_POINT ( 'NONE',  ( 94.79999999999995453, -35.00000000000000000, 150.0000000000000000 ) ) ;
#6874 = CARTESIAN_POINT ( 'NONE',  ( -84.51154815724953551, -35.14114861271051637, 98.22820072003833047 ) ) ;
#6875 = LINE ( 'NONE', #12728, #5859 ) ;
#6876 = EDGE_LOOP ( 'NONE', ( #6079, #11959, #17666, #18967, #16129, #2698, #4422, #1353 ) ) ;
#6877 = CARTESIAN_POINT ( 'NONE',  ( 232.5999999999999091, -32.08124999877096428, -47.00000000000011369 ) ) ;
#6878 = CARTESIAN_POINT ( 'NONE',  ( 235.4063471324517991, -34.99999999999999289, 99.92898555286095075 ) ) ;
#6879 = CYLINDRICAL_SURFACE ( 'NONE', #4907, 3.000000000000002665 ) ;
#6880 = CARTESIAN_POINT ( 'NONE',  ( 233.9782151781249411, -34.60312499938548569, 102.3871387122750889 ) ) ;
#6881 = CARTESIAN_POINT ( 'NONE',  ( -83.77821517812500929, -33.47812499938548569, 97.61286128772489690 ) ) ;
#6882 = CARTESIAN_POINT ( 'NONE',  ( 229.8435696437499303, -31.49062499938547788, -50.00000000000011369 ) ) ;
#6883 = ORIENTED_EDGE ( 'NONE', *, *, #6072, .F. ) ;
#6884 = CARTESIAN_POINT ( 'NONE',  ( 111.5000000000000142, 12.69999999999998508, 30.20101012677667285 ) ) ;
#6885 = CARTESIAN_POINT ( 'NONE',  ( -83.77821517812500929, -33.36562499938548854, 97.61286128772489690 ) ) ;
#6886 = CARTESIAN_POINT ( 'NONE',  ( -84.12112955302457351, -35.00000000000000000, -102.4658001909609908 ) ) ;
#6887 = CARTESIAN_POINT ( 'NONE',  ( 85.15643035624999868, -32.35312499938549280, 98.40857419181659793 ) ) ;
#6888 = CARTESIAN_POINT ( 'NONE',  ( 244.7999999999999545, -29.80000000000002203, 147.7999999999999829 ) ) ;
#6889 = CARTESIAN_POINT ( 'NONE',  ( 231.2217848218749339, -32.46562499938547575, -52.38713871227520968 ) ) ;
#6890 = CARTESIAN_POINT ( 'NONE',  ( -85.15643035625001289, -33.36562499938548854, 101.5914258081833879 ) ) ;
#6891 = CARTESIAN_POINT ( 'NONE',  ( -82.39999999999999147, -34.19062499938548427, -96.81714838363319586 ) ) ;
#6892 = CARTESIAN_POINT ( 'NONE',  ( 81.02178482187500208, -32.24062499938548854, 97.61286128772489690 ) ) ;
#6893 = CARTESIAN_POINT ( 'NONE',  ( 82.39999999999999147, -33.29062499938549280, -103.1828516163667899 ) ) ;
#6894 = EDGE_CURVE ( 'NONE', #1370, #9344, #18898, .T. ) ;
#6895 = CARTESIAN_POINT ( 'NONE',  ( 229.8435696437499303, -32.39062499938548001, -50.00000000000011369 ) ) ;
#6896 = CARTESIAN_POINT ( 'NONE',  ( -85.15643035625001289, -32.87812499938548427, 98.40857419181659793 ) ) ;
#6897 = CARTESIAN_POINT ( 'NONE',  ( 4.030859730898683324, -1.403482646610935358, -3.500000000000000000 ) ) ;
#6898 = VERTEX_POINT ( 'NONE', #17332 ) ;
#6899 = CARTESIAN_POINT ( 'NONE',  ( 83.77821517812500929, -34.37812499938548427, 102.3871387122750889 ) ) ;
#6900 = CARTESIAN_POINT ( 'NONE',  ( 231.7961524227065695, -32.34240381056765301, 96.99999999999998579 ) ) ;
#6901 = CARTESIAN_POINT ( 'NONE',  ( -83.90000000000000568, -34.42500000000000426, 102.5980762113533018 ) ) ;
#6902 =( BOUNDED_CURVE ( )  B_SPLINE_CURVE ( 2, ( #9433, #660, #12371, #9332, #7679, #562, #6519 ),
 .UNSPECIFIED., .F., .F. ) 
 B_SPLINE_CURVE_WITH_KNOTS ( ( 3, 2, 2, 3 ),
 ( 0.3702305174531566045, 0.3750000000000000000, 0.3888888888888888951, 0.3958333333333333148 ),
 .UNSPECIFIED. ) 
 CURVE ( )  GEOMETRIC_REPRESENTATION_ITEM ( )  RATIONAL_B_SPLINE_CURVE ( ( 0.9395835397633047759, 0.9539927561173232595, 1.000000000000000000, 0.8660254037844387076, 1.000000000000000000, 0.9330127018922196314, 0.9330127018922194093 ) ) 
 REPRESENTATION_ITEM ( '' )  );
#6903 = CARTESIAN_POINT ( 'NONE',  ( -83.77821517812500929, -31.56562499938548427, 97.61286128772489690 ) ) ;
#6904 = CARTESIAN_POINT ( 'NONE',  ( -81.02178482187500208, -31.34062499938548996, 102.3871387122750889 ) ) ;
#6905 = CARTESIAN_POINT ( 'NONE',  ( -82.40000000000000568, -30.00000000000000355, 96.99999999999998579 ) ) ;
#6906 = VERTEX_POINT ( 'NONE', #19184 ) ;
#6907 = CARTESIAN_POINT ( 'NONE',  ( -85.40000000000000568, -33.18750000000000000, -101.7320508075688679 ) ) ;
#6908 = LINE ( 'NONE', #12857, #1317 ) ;
#6909 = CARTESIAN_POINT ( 'NONE',  ( 232.5999999999999375, -32.81249999999999289, -53.00000000000011369 ) ) ;
#6910 = CARTESIAN_POINT ( 'NONE',  ( -85.40000000000000568, -30.89606250001229526, 99.99999999999998579 ) ) ;
#6911 = B_SPLINE_CURVE_WITH_KNOTS ( 'NONE', 3,
 ( #5639, #1047, #4068, #7000, #4166, #18734, #2793, #12953 ),
 .UNSPECIFIED., .F., .F.,
 ( 4, 2, 2, 4 ),
 ( 7.780516681398759253E-20, 0.002450665683189819696, 0.003675998524784729327, 0.004901331366379639391 ),
 .UNSPECIFIED. ) ;
#6912 = DIRECTION ( 'NONE',  ( -0.000000000000000000, -1.000000000000000000, -0.000000000000000000 ) ) ;
#6913 = LINE ( 'NONE', #17359, #2742 ) ;
#6914 = FACE_OUTER_BOUND ( 'NONE', #11258, .T. ) ;
#6915 = CARTESIAN_POINT ( 'NONE',  ( -81.59615242270660929, -32.32634618820329564, -102.9999999999999858 ) ) ;
#6916 = CARTESIAN_POINT ( 'NONE',  ( 4.000000000000000000, 2.309401076758497151, -3.433295621305379353 ) ) ;
#6917 = CARTESIAN_POINT ( 'NONE',  ( 230.8850348010513471, -31.99999999999999289, 97.81539907810714851 ) ) ;
#6918 = CARTESIAN_POINT ( 'NONE',  ( 232.5999999999999375, -32.98124999877095576, -47.00000000000011369 ) ) ;
#6919 = CARTESIAN_POINT ( 'NONE',  ( 82.39999999999999147, -33.96562499938548285, -96.81714838363319586 ) ) ;
#6920 = DIRECTION ( 'NONE',  ( 1.000000000000000000, 0.000000000000000000, -0.000000000000000000 ) ) ;
#6921 = ORIENTED_EDGE ( 'NONE', *, *, #18321, .T. ) ;
#6922 = CARTESIAN_POINT ( 'NONE',  ( 83.90000000000000568, -32.26874999877097139, 102.5980762113533018 ) ) ;
#6923 = CARTESIAN_POINT ( 'NONE',  ( 229.8435696437499871, -33.89062499938548001, 98.40857419181659793 ) ) ;
#6924 = CARTESIAN_POINT ( 'NONE',  ( 229.8435696437499303, -33.40312499938547575, -50.00000000000011369 ) ) ;
#6925 = CARTESIAN_POINT ( 'NONE',  ( 232.5999999999999091, -34.10624999877096286, 96.99999999999998579 ) ) ;
#6926 = CARTESIAN_POINT ( 'NONE',  ( 246.9999999999999716, -35.00000000000000000, -100.0000000000000000 ) ) ;
#6927 = ORIENTED_EDGE ( 'NONE', *, *, #3978, .T. ) ;
#6928 = CARTESIAN_POINT ( 'NONE',  ( -82.39999999999999147, -32.72812499938548569, -96.81714838363319586 ) ) ;
#6929 = CARTESIAN_POINT ( 'NONE',  ( 79.39999999999999147, -32.41874999877096997, 99.99999999999998579 ) ) ;
#6930 = VERTEX_POINT ( 'NONE', #2766 ) ;
#6931 = CARTESIAN_POINT ( 'NONE',  ( 82.39999999999999147, -32.61562499938548854, 103.1828516163667899 ) ) ;
#6932 = CARTESIAN_POINT ( 'NONE',  ( -83.77821517812500929, -31.07812499938548711, -97.61286128772489690 ) ) ;
#6933 = CARTESIAN_POINT ( 'NONE',  ( 79.39999999999999147, -33.33749999999999858, 101.7320508075688821 ) ) ;
#6934 = CARTESIAN_POINT ( 'NONE',  ( 235.3564303562499447, -30.44062499938548072, 98.40857419181659793 ) ) ;
#6935 = CARTESIAN_POINT ( 'NONE',  ( -80.90000000000000568, -35.04374999877096997, 97.40192378864668399 ) ) ;
#6936 = CARTESIAN_POINT ( 'NONE',  ( -82.39999999999999147, -35.23124999877096997, 103.4641016151377499 ) ) ;
#6937 = CARTESIAN_POINT ( 'NONE',  ( -85.15643035625001289, -33.25312499938548427, -98.40857419181659793 ) ) ;
#6938 = VECTOR ( 'NONE', #8521, 1000.000000000000000 ) ;
#6939 = CARTESIAN_POINT ( 'NONE',  ( -82.40000000000000568, -30.00000000000000355, 103.0000000000000000 ) ) ;
#6940 = CARTESIAN_POINT ( 'NONE',  ( 80.90000000000000568, -30.99374999877096926, -97.40192378864668399 ) ) ;
#6941 = CARTESIAN_POINT ( 'NONE',  ( 235.5999999999999943, -30.63749999999999574, 98.26794919243110371 ) ) ;
#6942 = ORIENTED_EDGE ( 'NONE', *, *, #1842, .F. ) ;
#6943 = CARTESIAN_POINT ( 'NONE',  ( 79.64356964374999848, -33.96562499938548285, -99.99999999999998579 ) ) ;
#6944 = CARTESIAN_POINT ( 'NONE',  ( 231.0999999999999375, -33.91874999877096286, 102.5980762113533018 ) ) ;
#6945 = CARTESIAN_POINT ( 'NONE',  ( -82.40000000000001990, -32.53124999877097423, -97.00000000000000000 ) ) ;
#6946 = EDGE_LOOP ( 'NONE', ( #2390, #8409, #18294, #7255 ) ) ;
#6947 = EDGE_CURVE ( 'NONE', #17768, #11098, #294, .T. ) ;
#6948 = CARTESIAN_POINT ( 'NONE',  ( -85.15643035625001289, -31.04062499938548569, 99.99999999999998579 ) ) ;
#6949 = DIRECTION ( 'NONE',  ( 0.000000000000000000, 0.000000000000000000, -1.000000000000000000 ) ) ;
#6950 = VERTEX_POINT ( 'NONE', #11466 ) ;
#6951 = CARTESIAN_POINT ( 'NONE',  ( 4.086376042167606748, -1.979461949354205164, 3.571471332069182658 ) ) ;
#6952 = CIRCLE ( 'NONE', #9429, 3.500000000000000000 ) ;
#6953 = AXIS2_PLACEMENT_3D ( 'NONE', #7386, #14908, #1625 ) ;
#6954 = EDGE_LOOP ( 'NONE', ( #2366, #6561, #8406, #13956 ) ) ;
#6955 = CARTESIAN_POINT ( 'NONE',  ( 94.79999999999995453, -35.00000000000000000, 150.0000000000000000 ) ) ;
#6956 = CARTESIAN_POINT ( 'NONE',  ( 82.39999999999999147, -32.58750000000000568, -103.4641016151377499 ) ) ;
#6957 = DIRECTION ( 'NONE',  ( 2.312964634635736745E-15, 1.000000000000000000, 0.000000000000000000 ) ) ;
#6958 = CARTESIAN_POINT ( 'NONE',  ( -85.15643035624999868, -32.09062499938548996, 98.40857419181659793 ) ) ;
#6959 = CARTESIAN_POINT ( 'NONE',  ( -79.39999999999999147, -32.88750000000000284, 98.26794919243110371 ) ) ;
#6960 = CARTESIAN_POINT ( 'NONE',  ( 99.99999999999994316, -21.80000000000003268, -142.6499999999999773 ) ) ;
#6961 = CARTESIAN_POINT ( 'NONE',  ( 231.0999999999999375, -32.11874999877096570, -47.40192378864679768 ) ) ;
#6962 = APPLICATION_CONTEXT ( 'automotive_design' ) ;
#6963 = DIRECTION ( 'NONE',  ( 0.000000000000000000, 0.000000000000000000, -1.000000000000000000 ) ) ;
#6964 = CARTESIAN_POINT ( 'NONE',  ( 0.02993401039713615083, 3.373851915354614928, 1.156317065392238774 ) ) ;
#6965 = VECTOR ( 'NONE', #11126, 1000.000000000000000 ) ;
#6966 = CARTESIAN_POINT ( 'NONE',  ( 109.9999999999999858, -1.546382070013610932E-13, -2.407412430484045937E-29 ) ) ;
#6967 = VERTEX_POINT ( 'NONE', #16056 ) ;
#6968 = CARTESIAN_POINT ( 'NONE',  ( 232.5999999999999375, -34.61249999999999716, -53.46410161513786363 ) ) ;
#6969 = CARTESIAN_POINT ( 'NONE',  ( 85.40000000000000568, -34.93124999877096570, 101.7320508075688821 ) ) ;
#6970 = CARTESIAN_POINT ( 'NONE',  ( -82.40000000000001990, -33.93750000000000711, 103.0000000000000000 ) ) ;
#6971 = CARTESIAN_POINT ( 'NONE',  ( -81.02178482187500208, -32.65312499938548996, 97.61286128772489690 ) ) ;
#6972 = CARTESIAN_POINT ( 'NONE',  ( 229.8435696437499303, -35.20312499938548001, -50.00000000000011369 ) ) ;
#6973 = ADVANCED_FACE ( 'NONE', ( #8621 ), #5800, .F. ) ;
#6974 = VERTEX_POINT ( 'NONE', #10293 ) ;
#6975 = CARTESIAN_POINT ( 'NONE',  ( -79.64356964375001269, -34.00312499938549138, 101.5914258081833879 ) ) ;
#6976 = CARTESIAN_POINT ( 'NONE',  ( -79.39999999999999147, -30.58124999877096784, 98.26794919243110371 ) ) ;
#6977 = CARTESIAN_POINT ( 'NONE',  ( 85.15643035624999868, -34.22812499938547859, 101.5914258081833879 ) ) ;
#6978 = CYLINDRICAL_SURFACE ( 'NONE', #6501, 3.000000000000002665 ) ;
#6979 = DIRECTION ( 'NONE',  ( -0.000000000000000000, -1.000000000000000000, -0.000000000000000000 ) ) ;
#6980 = CARTESIAN_POINT ( 'NONE',  ( -79.64356964374998427, -34.04062499938549280, 98.40857419181659793 ) ) ;
#6981 = CARTESIAN_POINT ( 'NONE',  ( -83.77821517812500929, -34.82812499938548711, -102.3871387122750889 ) ) ;
#6982 = CARTESIAN_POINT ( 'NONE',  ( 79.64356964374999848, -32.16562499938548569, 99.99999999999998579 ) ) ;
#6983 = EDGE_CURVE ( 'NONE', #4985, #14591, #6645, .T. ) ;
#6984 = CARTESIAN_POINT ( 'NONE',  ( 85.15643035624999868, -33.36562499938548854, -101.5914258081833879 ) ) ;
#6985 = CARTESIAN_POINT ( 'NONE',  ( 231.2217848218749339, -32.46562499938547575, -52.38713871227520968 ) ) ;
#6986 = CARTESIAN_POINT ( 'NONE',  ( -83.77821517812500929, -32.91562499938547859, 97.61286128772489690 ) ) ;
#6987 = CARTESIAN_POINT ( 'NONE',  ( 82.39999999999999147, -30.25312499938548783, -96.81714838363319586 ) ) ;
#6988 = ADVANCED_FACE ( 'NONE', ( #3941 ), #18885, .F. ) ;
#6989 = ORIENTED_EDGE ( 'NONE', *, *, #13471, .F. ) ;
#6990 = DIRECTION ( 'NONE',  ( -0.000000000000000000, -1.000000000000000000, -0.000000000000000000 ) ) ;
#6991 = CARTESIAN_POINT ( 'NONE',  ( 232.5999999999999375, -32.36249999999999716, 97.00000000000000000 ) ) ;
#6992 = CARTESIAN_POINT ( 'NONE',  ( -85.40000000000000568, -34.01250000000000284, 101.7320508075688679 ) ) ;
#6993 = CARTESIAN_POINT ( 'NONE',  ( -85.15643035624999868, -33.70312499938548711, 101.5914258081833879 ) ) ;
#6994 = CARTESIAN_POINT ( 'NONE',  ( -81.02178482187500208, -30.44062499938548783, 102.3871387122750889 ) ) ;
#6995 = DIRECTION ( 'NONE',  ( 0.000000000000000000, 0.000000000000000000, 1.000000000000000000 ) ) ;
#6996 = CARTESIAN_POINT ( 'NONE',  ( 229.8435696437499587, -32.87812499938547717, 98.40857419181659793 ) ) ;
#6997 = DIRECTION ( 'NONE',  ( 0.000000000000000000, 0.000000000000000000, -1.000000000000000000 ) ) ;
#6998 = EDGE_CURVE ( 'NONE', #7789, #3915, #5177, .T. ) ;
#6999 = CARTESIAN_POINT ( 'NONE',  ( -79.39999999999999147, -30.18356250001229313, 98.26794919243110371 ) ) ;
#7000 = CARTESIAN_POINT ( 'NONE',  ( 2.449848172108560096, 3.432307619358740514, -3.503702292528905637 ) ) ;
#7001 = DIRECTION ( 'NONE',  ( 0.000000000000000000, 0.000000000000000000, -1.000000000000000000 ) ) ;
#7002 = CARTESIAN_POINT ( 'NONE',  ( -79.64356964375001269, -30.77812499938548285, 98.40857419181659793 ) ) ;
#7003 = DIRECTION ( 'NONE',  ( -0.000000000000000000, -1.000000000000000000, -0.000000000000000000 ) ) ;
#7004 = CARTESIAN_POINT ( 'NONE',  ( 4.000000000000000000, -1.084202172485504434E-14, -3.142992957459231906 ) ) ;
#7005 = CARTESIAN_POINT ( 'NONE',  ( 235.4117376914898045, -31.99999999999999289, 98.95399275611721635 ) ) ;
#7006 = DIRECTION ( 'NONE',  ( 0.000000000000000000, 0.000000000000000000, -1.000000000000000000 ) ) ;
#7007 = CARTESIAN_POINT ( 'NONE',  ( 79.64356964375001269, -32.76562499938548711, -101.5914258081833879 ) ) ;
#7008 = CARTESIAN_POINT ( 'NONE',  ( -83.90000000000000568, -33.16874999877096286, 97.40192378864668399 ) ) ;
#7009 = ORIENTED_EDGE ( 'NONE', *, *, #7442, .T. ) ;
#7010 = CARTESIAN_POINT ( 'NONE',  ( 80.90000000000000568, -32.94374999877096855, 97.40192378864668399 ) ) ;
#7011 = B_SPLINE_CURVE_WITH_KNOTS ( 'NONE', 3,
 ( #8426, #7249, #10091, #17427, #11743 ),
 .UNSPECIFIED., .F., .F.,
 ( 4, 1, 4 ),
 ( 0.000000000000000000, 0.002309401076758505356, 0.004618802153517010713 ),
 .UNSPECIFIED. ) ;
#7012 = LINE ( 'NONE', #10041, #3658 ) ;
#7013 = EDGE_CURVE ( 'NONE', #9852, #17568, #6010, .T. ) ;
#7014 = CARTESIAN_POINT ( 'NONE',  ( 229.8435696437499871, -33.36562499938548143, -48.40857419181671162 ) ) ;
#7015 = CARTESIAN_POINT ( 'NONE',  ( 85.40000000000000568, -34.46249999999999858, 98.26794919243111792 ) ) ;
#7016 = DIRECTION ( 'NONE',  ( -1.586032892321652088E-15, -1.000000000000000000, 0.000000000000000000 ) ) ;
#7017 = ORIENTED_EDGE ( 'NONE', *, *, #14847, .T. ) ;
#7018 = CARTESIAN_POINT ( 'NONE',  ( -85.15643035624999868, -35.05312499938548143, -98.40857419181659793 ) ) ;
#7019 = DIRECTION ( 'NONE',  ( 7.222237291452147586E-32, -1.214306433183764966E-16, 1.000000000000000000 ) ) ;
#7020 = VERTEX_POINT ( 'NONE', #6264 ) ;
#7021 = CARTESIAN_POINT ( 'NONE',  ( 85.15643035625001289, -33.36562499938548854, 98.40857419181659793 ) ) ;
#7022 = EDGE_CURVE ( 'NONE', #11515, #12396, #16882, .T. ) ;
#7023 = CARTESIAN_POINT ( 'NONE',  ( -81.02178482187500208, -31.00312499938548783, -97.61286128772489690 ) ) ;
#7024 = CARTESIAN_POINT ( 'NONE',  ( 80.90000000000000568, -33.75000000000000000, 102.5980762113533018 ) ) ;
#7025 = CARTESIAN_POINT ( 'NONE',  ( 229.8435696437499303, -30.25312499938548072, 99.99999999999998579 ) ) ;
#7026 = CARTESIAN_POINT ( 'NONE',  ( -85.40000000000000568, -34.93124999877096570, 98.26794919243111792 ) ) ;
#7027 = CARTESIAN_POINT ( 'NONE',  ( -85.15643035624999868, -32.09062499938548996, 98.40857419181659793 ) ) ;
#7028 = CARTESIAN_POINT ( 'NONE',  ( -82.39999999999999147, -33.17812499938548854, -96.81714838363319586 ) ) ;
#7029 = VECTOR ( 'NONE', #282, 1000.000000000000000 ) ;
#7030 = CARTESIAN_POINT ( 'NONE',  ( 233.2099102960629011, -35.00000000000001421, 102.6939647107543010 ) ) ;
#7031 = CARTESIAN_POINT ( 'NONE',  ( 85.40000000000000568, -31.78124999877096712, -98.26794919243111792 ) ) ;
#7032 = CARTESIAN_POINT ( 'NONE',  ( 234.0999999999999375, -31.94999999999999218, 97.40192378864668399 ) ) ;
#7033 = ORIENTED_EDGE ( 'NONE', *, *, #6872, .T. ) ;
#7034 = CYLINDRICAL_SURFACE ( 'NONE', #15365, 5.199999999999996625 ) ;
#7035 = CARTESIAN_POINT ( 'NONE',  ( 231.0999999999999375, -33.01874999877096428, 102.5980762113533018 ) ) ;
#7036 = CARTESIAN_POINT ( 'NONE',  ( 229.5999999999999375, -30.80624999877096215, -48.26794919243123161 ) ) ;
#7037 = CARTESIAN_POINT ( 'NONE',  ( 229.5999999999999375, -34.53749999999999432, 98.26794919243111792 ) ) ;
#7038 = CARTESIAN_POINT ( 'NONE',  ( -82.39999999999999147, -31.37812499938548427, 103.1828516163667899 ) ) ;
#7039 = VERTEX_POINT ( 'NONE', #6648 ) ;
#7040 = ORIENTED_EDGE ( 'NONE', *, *, #8764, .T. ) ;
#7041 = VECTOR ( 'NONE', #8531, 1000.000000000000000 ) ;
#7042 = CARTESIAN_POINT ( 'NONE',  ( -85.40000000000000568, -32.19374999877096855, 99.99999999999998579 ) ) ;
#7043 = ORIENTED_EDGE ( 'NONE', *, *, #12020, .T. ) ;
#7044 = CARTESIAN_POINT ( 'NONE',  ( 85.40000000000000568, -32.28750000000000142, -98.26794919243111792 ) ) ;
#7045 = CARTESIAN_POINT ( 'NONE',  ( 84.12306224665901766, -31.99999999999999289, -102.1915028381726529 ) ) ;
#7046 = CARTESIAN_POINT ( 'NONE',  ( -81.02178482187500208, -32.65312499938548996, 97.61286128772489690 ) ) ;
#7047 = CARTESIAN_POINT ( 'NONE',  ( -80.90000000000000568, -31.65000000000000568, 102.5980762113533018 ) ) ;
#7048 = CARTESIAN_POINT ( 'NONE',  ( -82.40000000000000568, -34.10624999877096997, 96.99999999999998579 ) ) ;
#7049 = CARTESIAN_POINT ( 'NONE',  ( 230.8850348010514892, -31.99999999999999289, -52.18460092189305755 ) ) ;
#7050 = B_SPLINE_CURVE_WITH_KNOTS ( 'NONE', 3,
 ( #17551, #14319, #6716, #4167, #958, #2592 ),
 .UNSPECIFIED., .F., .F.,
 ( 4, 2, 4 ),
 ( -3.640115492407174633E-06, 0.0002066546034003413743, 0.0004169493222930899571 ),
 .UNSPECIFIED. ) ;
#7051 = CARTESIAN_POINT ( 'NONE',  ( 85.40000000000000568, -34.03124999877096712, 101.7320508075688821 ) ) ;
#7052 = CARTESIAN_POINT ( 'NONE',  ( -84.70833260042415702, -35.00006955123599539, 98.08383195543535749 ) ) ;
#7053 = DIRECTION ( 'NONE',  ( 0.000000000000000000, 0.000000000000000000, 1.000000000000000000 ) ) ;
#7054 = CARTESIAN_POINT ( 'NONE',  ( 94.79999999999991189, -3.000000000000000000, 150.0000000000000000 ) ) ;
#7055 = EDGE_LOOP ( 'NONE', ( #2733, #15053, #5964, #16151 ) ) ;
#7056 = CARTESIAN_POINT ( 'NONE',  ( -85.15643035624999868, -30.62812499938548427, -101.5914258081833879 ) ) ;
#7057 = DIRECTION ( 'NONE',  ( -0.000000000000000000, -1.000000000000000000, -0.000000000000000000 ) ) ;
#7058 = CARTESIAN_POINT ( 'NONE',  ( -1.360585162435467455, 4.061296242128285883, -3.505054077164959203 ) ) ;
#7059 = CARTESIAN_POINT ( 'NONE',  ( 235.3564303562499447, -33.59062499938547575, 98.40857419181659793 ) ) ;
#7060 = CARTESIAN_POINT ( 'NONE',  ( -82.39999999999999147, -33.96562499938548285, 96.81714838363319586 ) ) ;
#7061 = DIRECTION ( 'NONE',  ( -0.6427825299241916035, 4.877271974511416535E-06, 0.7660487055014636448 ) ) ;
#7062 = CARTESIAN_POINT ( 'NONE',  ( 233.9782151781249411, -30.44062499938548072, -47.61286128772501769 ) ) ;
#7063 = ORIENTED_EDGE ( 'NONE', *, *, #13529, .T. ) ;
#7064 = CARTESIAN_POINT ( 'NONE',  ( -79.64356964375001269, -33.92812499938548854, 98.40857419181659793 ) ) ;
#7065 = PRESENTATION_LAYER_ASSIGNMENT (  '', '', ( #13965 ) ) ;
#7066 = CARTESIAN_POINT ( 'NONE',  ( -82.85024983566745505, -35.00000000000000711, -102.9730910282409440 ) ) ;
#7068 = CARTESIAN_POINT ( 'NONE',  ( 85.15643035625001289, -33.74062499938548854, 99.99999999999998579 ) ) ;
#7067 = APPLICATION_CONTEXT ( 'automotive_design' ) ;
#7069 = CARTESIAN_POINT ( 'NONE',  ( 235.3564303562499447, -32.61562499938548143, 99.99999999999998579 ) ) ;
#7070 = FACE_OUTER_BOUND ( 'NONE', #4688, .T. ) ;
#7071 = CARTESIAN_POINT ( 'NONE',  ( -81.02178482187500208, -34.15312499938548285, 102.3871387122750889 ) ) ;
#7072 = CARTESIAN_POINT ( 'NONE',  ( -79.64356964374998427, -33.66562499938548569, -98.40857419181659793 ) ) ;
#7073 = CARTESIAN_POINT ( 'NONE',  ( 5.599999999999998757, 0.000000000000000000, 0.000000000000000000 ) ) ;
#7074 = EDGE_CURVE ( 'NONE', #4275, #10919, #5427, .T. ) ;
#7075 = PRODUCT_DEFINITION_FORMATION_WITH_SPECIFIED_SOURCE ( 'ANY', '', #19045, .NOT_KNOWN. ) ;
#7076 = EDGE_CURVE ( 'NONE', #10346, #10326, #1854, .T. ) ;
#7077 = CARTESIAN_POINT ( 'NONE',  ( 85.15643035624999868, -34.71562499938548285, -101.5914258081833879 ) ) ;
#7078 = CARTESIAN_POINT ( 'NONE',  ( 229.8435696437499871, -34.22812499938547148, -51.59142580818350865 ) ) ;
#7079 = CARTESIAN_POINT ( 'NONE',  ( -85.15643035625001289, -33.32812499938548711, 98.40857419181659793 ) ) ;
#7080 = CARTESIAN_POINT ( 'NONE',  ( 83.77821517812500929, -32.01562499938548001, -97.61286128772489690 ) ) ;
#7081 = VERTEX_POINT ( 'NONE', #2149 ) ;
#7082 = CARTESIAN_POINT ( 'NONE',  ( 25.60000000000000142, 0.000000000000000000, 0.000000000000000000 ) ) ;
#7083 = CARTESIAN_POINT ( 'NONE',  ( 233.4038475772933054, -34.12634618820329280, -53.00000000000012790 ) ) ;
#7084 = CARTESIAN_POINT ( 'NONE',  ( -83.90000000000000568, -32.77499999999999858, 97.40192378864668399 ) ) ;
#7085 = CARTESIAN_POINT ( 'NONE',  ( -81.02178482187500208, -34.34062499938548285, 97.61286128772489690 ) ) ;
#7086 = CARTESIAN_POINT ( 'NONE',  ( -85.15643035625001289, -31.49062499938548498, 99.99999999999998579 ) ) ;
#7087 = ORIENTED_EDGE ( 'NONE', *, *, #1328, .F. ) ;
#7088 = CYLINDRICAL_SURFACE ( 'NONE', #17431, 3.000000000000009770 ) ;
#7089 = AXIS2_PLACEMENT_3D ( 'NONE', #4511, #18386, #13870 ) ;
#7090 = EDGE_CURVE ( 'NONE', #1776, #711, #18179, .T. ) ;
#7091 = CARTESIAN_POINT ( 'NONE',  ( 233.9782151781249411, -33.14062499938548001, 102.3871387122750889 ) ) ;
#7092 = CARTESIAN_POINT ( 'NONE',  ( 81.48596794228853923, -34.99999999999999289, -97.18639806692210925 ) ) ;
#7093 = FACE_OUTER_BOUND ( 'NONE', #14807, .T. ) ;
#7094 = AXIS2_PLACEMENT_3D ( 'NONE', #16482, #3086, #10328 ) ;
#7095 = CARTESIAN_POINT ( 'NONE',  ( 3.972066048304737418, 2.740530939476172989, -2.384802634787877018 ) ) ;
#7096 = CARTESIAN_POINT ( 'NONE',  ( -83.95700771753406855, -35.00000000000000711, 97.42750194505822492 ) ) ;
#7097 = CARTESIAN_POINT ( 'NONE',  ( 4.175813232069146785, 2.061359961916366057, -3.570380186727397653 ) ) ;
#7098 = CARTESIAN_POINT ( 'NONE',  ( -83.20384757729335945, -33.69240381056766154, 96.99999999999998579 ) ) ;
#7099 = CARTESIAN_POINT ( 'NONE',  ( -83.20384757729333103, -33.18615380933863435, -103.0000000000000000 ) ) ;
#7100 = EDGE_CURVE ( 'NONE', #1155, #2812, #1538, .T. ) ;
#7101 = CARTESIAN_POINT ( 'NONE',  ( 232.5999999999999091, -32.08124999877096428, 102.9999999999999858 ) ) ;
#7102 = VECTOR ( 'NONE', #9191, 1000.000000000000000 ) ;
#7103 = CARTESIAN_POINT ( 'NONE',  ( -85.40000000000000568, -32.60624999877096997, -98.26794919243111792 ) ) ;
#7104 = CARTESIAN_POINT ( 'NONE',  ( 85.15643035624999868, -33.44062499938548427, -98.40857419181659793 ) ) ;
#7105 = CARTESIAN_POINT ( 'NONE',  ( 231.7961524227065695, -34.14240381056765017, 96.99999999999998579 ) ) ;
#7106 = ORIENTED_EDGE ( 'NONE', *, *, #11374, .F. ) ;
#7107 = CARTESIAN_POINT ( 'NONE',  ( 85.40000000000000568, -32.15624999877096712, 98.26794919243111792 ) ) ;
#7108 = CARTESIAN_POINT ( 'NONE',  ( 231.2217848218749339, -34.37812499938547717, 97.61286128772489690 ) ) ;
#7109 = CARTESIAN_POINT ( 'NONE',  ( 233.9782151781249411, -35.05312499938548143, -47.61286128772501769 ) ) ;
#7110 = AXIS2_PLACEMENT_3D ( 'NONE', #26, #1581, #13393 ) ;
#7111 = STYLED_ITEM ( 'NONE', ( #4413 ), #14131 ) ;
#7112 = CARTESIAN_POINT ( 'NONE',  ( -79.64356964375001269, -34.90312499938548285, 101.5914258081833879 ) ) ;
#7113 = CARTESIAN_POINT ( 'NONE',  ( -84.25709831968909214, -35.00000000000001421, -97.88253972981382844 ) ) ;
#7114 = ORIENTED_EDGE ( 'NONE', *, *, #12808, .T. ) ;
#7115 = CARTESIAN_POINT ( 'NONE',  ( -81.02178482187500208, -33.44062499938548427, -102.3871387122750889 ) ) ;
#7116 = CARTESIAN_POINT ( 'NONE',  ( 81.59615242270660929, -32.32634618820329564, 102.9999999999999858 ) ) ;
#7117 = EDGE_LOOP ( 'NONE', ( #5060, #157, #5898, #9953 ) ) ;
#7118 = CARTESIAN_POINT ( 'NONE',  ( -82.40000000000000568, -30.00000000000000355, -99.99999999999998579 ) ) ;
#7119 = AXIS2_PLACEMENT_3D ( 'NONE', #15789, #9730, #15694 ) ;
#7120 = CARTESIAN_POINT ( 'NONE',  ( -81.02178482187500208, -30.40312499938548640, -102.3871387122750889 ) ) ;
#7121 = CARTESIAN_POINT ( 'NONE',  ( -79.39999999999999147, -30.58124999877096784, -101.7320508075688821 ) ) ;
#7122 = CARTESIAN_POINT ( 'NONE',  ( -81.48596794228825502, -35.00000000000001421, 97.18639806692218031 ) ) ;
#7123 = CARTESIAN_POINT ( 'NONE',  ( -79.39999999999999147, -33.76874999877097139, 99.99999999999998579 ) ) ;
#7124 = CARTESIAN_POINT ( 'NONE',  ( -81.02178482187500208, -30.85312499938548569, 97.61286128772489690 ) ) ;
#7125 = AXIS2_PLACEMENT_3D ( 'NONE', #9203, #15168, #4729 ) ;
#7126 = CARTESIAN_POINT ( 'NONE',  ( -81.02178482187500208, -32.69062499938548427, -97.61286128772489690 ) ) ;
#7127 = CARTESIAN_POINT ( 'NONE',  ( -79.39999999999999147, -34.25624999877096855, -98.26794919243113213 ) ) ;
#7128 = CARTESIAN_POINT ( 'NONE',  ( 83.90000000000000568, -31.81874999877096855, -97.40192378864668399 ) ) ;
#7129 = CARTESIAN_POINT ( 'NONE',  ( 231.0999999999999375, -31.42499999999999361, 97.40192378864668399 ) ) ;
#7130 = ORIENTED_EDGE ( 'NONE', *, *, #15919, .T. ) ;
#7131 = CARTESIAN_POINT ( 'NONE',  ( 85.15643035625001289, -34.22812499938548569, -98.40857419181659793 ) ) ;
#7132 =( LENGTH_UNIT ( ) NAMED_UNIT ( * ) SI_UNIT ( .MILLI., .METRE. ) );
#7133 = EDGE_CURVE ( 'NONE', #6130, #14453, #3604, .T. ) ;
#7134 = CARTESIAN_POINT ( 'NONE',  ( 231.0999999999999375, -33.16874999877095576, 97.40192378864668399 ) ) ;
#7135 = CARTESIAN_POINT ( 'NONE',  ( -96.99999999999998579, 0.000000000000000000, 150.0000000000000000 ) ) ;
#7136 = FACE_OUTER_BOUND ( 'NONE', #5682, .T. ) ;
#7137 = CARTESIAN_POINT ( 'NONE',  ( -83.77821517812500929, -31.41562499938548569, 102.3871387122750889 ) ) ;
#7138 = ORIENTED_EDGE ( 'NONE', *, *, #14831, .F. ) ;
#7139 = EDGE_LOOP ( 'NONE', ( #18390, #8923, #18174, #9009 ) ) ;
#7140 = LINE ( 'NONE', #16412, #12255 ) ;
#7141 = CIRCLE ( 'NONE', #3702, 5.199999999999996625 ) ;
#7142 = CARTESIAN_POINT ( 'NONE',  ( 3.972709601346591235, 2.746729940827189242, -2.374099244652734697 ) ) ;
#7143 = EDGE_LOOP ( 'NONE', ( #2243, #16176, #2352, #12996 ) ) ;
#7144 = CARTESIAN_POINT ( 'NONE',  ( 81.59615242270660929, -32.32634618820329564, -96.99999999999997158 ) ) ;
#7145 = CARTESIAN_POINT ( 'NONE',  ( 85.40000000000000568, -33.18750000000000000, -98.26794919243111792 ) ) ;
#7146 = LINE ( 'NONE', #19067, #1751 ) ;
#7147 = CARTESIAN_POINT ( 'NONE',  ( -79.64356964375001269, -30.96562499938548640, 101.5914258081833879 ) ) ;
#7148 = CARTESIAN_POINT ( 'NONE',  ( -79.39999999999999147, -32.47500000000000142, 99.99999999999998579 ) ) ;
#7149 = LINE ( 'NONE', #9987, #16485 ) ;
#7150 =( NAMED_UNIT ( * ) SI_UNIT ( $, .STERADIAN. ) SOLID_ANGLE_UNIT ( ) );
#7151 = B_SPLINE_CURVE_WITH_KNOTS ( 'NONE', 3,
 ( #9220, #17044, #12262, #15582, #13907, #545, #4941, #1898, #12355, #15283, #15184, #15482, #7860, #18322, #646, #6401 ),
 .UNSPECIFIED., .F., .F.,
 ( 4, 2, 2, 2, 2, 2, 2, 4 ),
 ( 0.000000000000000000, 0.0005391024520904644192, 0.001078204904180928838, 0.002156409808361877192, 0.002695512260452351695, 0.003234614712542825329, 0.003773717164633299398, 0.004312819616723773467 ),
 .UNSPECIFIED. ) ;
#7152 = CARTESIAN_POINT ( 'NONE',  ( 232.5999999999999375, -33.26249999999999574, 97.00000000000000000 ) ) ;
#7153 = DIRECTION ( 'NONE',  ( 1.000000000000000000, 0.000000000000000000, -0.000000000000000000 ) ) ;
#7154 = CARTESIAN_POINT ( 'NONE',  ( -83.20384757729338787, -34.59240381056766722, -102.9999999999999858 ) ) ;
#7155 = ORIENTED_EDGE ( 'NONE', *, *, #6894, .T. ) ;
#7156 =( NAMED_UNIT ( * ) PLANE_ANGLE_UNIT ( ) SI_UNIT ( $, .RADIAN. ) );
#7157 = CARTESIAN_POINT ( 'NONE',  ( -85.15643035625001289, -30.59062499938548285, -99.99999999999998579 ) ) ;
#7158 = CARTESIAN_POINT ( 'NONE',  ( 232.3466685930879123, -34.99995246259152282, 97.01071553687879145 ) ) ;
#7159 = CARTESIAN_POINT ( 'NONE',  ( 4.050880675075948290, -1.379097446046192887, -3.567934390854430760 ) ) ;
#7160 = CARTESIAN_POINT ( 'NONE',  ( 232.5999999999999943, -34.64062499938548001, 103.1828516163667899 ) ) ;
#7161 = CARTESIAN_POINT ( 'NONE',  ( -84.51154815724953551, -35.25364861271051353, 98.22820072003833047 ) ) ;
#7162 = CARTESIAN_POINT ( 'NONE',  ( 79.39999999999999147, -32.47500000000000142, 99.99999999999998579 ) ) ;
#7163 = CARTESIAN_POINT ( 'NONE',  ( 235.3564303562499447, -32.16562499938547859, -50.00000000000011369 ) ) ;
#7164 = ORIENTED_EDGE ( 'NONE', *, *, #6746, .T. ) ;
#7165 = CARTESIAN_POINT ( 'NONE',  ( -85.15643035624999868, -33.77812499938548285, 98.40857419181659793 ) ) ;
#7166 = CARTESIAN_POINT ( 'NONE',  ( -79.39999999999999147, -30.65624999877096712, 101.7320508075688537 ) ) ;
#7167 = CARTESIAN_POINT ( 'NONE',  ( 82.39999999999999147, -30.56250000000000355, 103.4641016151377499 ) ) ;
#7168 = EDGE_CURVE ( 'NONE', #15956, #10850, #10197, .T. ) ;
#7169 = DIRECTION ( 'NONE',  ( -0.000000000000000000, -1.000000000000000000, -0.000000000000000000 ) ) ;
#7170 = CARTESIAN_POINT ( 'NONE',  ( 233.9782151781249411, -30.29062499938547859, 97.61286128772489690 ) ) ;
#7171 = CARTESIAN_POINT ( 'NONE',  ( 233.9782151781249411, -32.69062499938547717, -47.61286128772501769 ) ) ;
#7172 = CARTESIAN_POINT ( 'NONE',  ( -79.64356964374999848, -34.07812499938548711, -99.99999999999998579 ) ) ;
#7173 = CARTESIAN_POINT ( 'NONE',  ( 83.77821517812500929, -34.71562499938548285, 102.3871387122750889 ) ) ;
#7174 = CARTESIAN_POINT ( 'NONE',  ( 82.39999999999999147, -32.05312499938548854, -96.81714838363319586 ) ) ;
#7175 = CARTESIAN_POINT ( 'NONE',  ( 229.5999999999999375, -30.41249999999999076, -48.26794919243123161 ) ) ;
#7176 = CARTESIAN_POINT ( 'NONE',  ( -82.39999999999999147, -33.40312499938548285, 96.81714838363319586 ) ) ;
#7177 = CARTESIAN_POINT ( 'NONE',  ( 4.086375874528100027, -2.103253014742892280, -3.500000000000000000 ) ) ;
#7178 = ORIENTED_EDGE ( 'NONE', *, *, #4144, .T. ) ;
#7179 = FACE_OUTER_BOUND ( 'NONE', #8186, .T. ) ;
#7180 = LINE ( 'NONE', #15975, #10856 ) ;
#7181 = CARTESIAN_POINT ( 'NONE',  ( 231.2217848218749339, -31.22812499938547859, -52.38713871227520968 ) ) ;
#7182 = CARTESIAN_POINT ( 'NONE',  ( -79.64356964375001269, -33.02812499938548285, 98.40857419181659793 ) ) ;
#7183 = ORIENTED_EDGE ( 'NONE', *, *, #6023, .T. ) ;
#7184 = CARTESIAN_POINT ( 'NONE',  ( -85.40000000000000568, -30.41249999999999787, 101.7320508075688821 ) ) ;
#7185 = CARTESIAN_POINT ( 'NONE',  ( 232.5999999999999943, -32.27812499938547575, 103.1828516163667899 ) ) ;
#7186 = CARTESIAN_POINT ( 'NONE',  ( 105.1999999999999602, -35.00000000000000711, -97.80000000000002558 ) ) ;
#7187 = CARTESIAN_POINT ( 'NONE',  ( 85.40000000000000568, -33.60000000000000142, -99.99999999999998579 ) ) ;
#7188 = CARTESIAN_POINT ( 'NONE',  ( 4.180345304246197102, 2.049116244671343345, -3.591763845239307251 ) ) ;
#7189 = CARTESIAN_POINT ( 'NONE',  ( 234.5796347213265278, -32.00000000000000000, -47.80162405160952233 ) ) ;
#7190 = CARTESIAN_POINT ( 'NONE',  ( -81.02178482187500208, -32.09062499938548285, 97.61286128772489690 ) ) ;
#7191 = DIRECTION ( 'NONE',  ( 1.000000000000000000, -1.387778780781445676E-15, -2.407412430484046130E-31 ) ) ;
#7192 = CARTESIAN_POINT ( 'NONE',  ( 79.64356964375001269, -33.66562499938549280, 98.40857419181659793 ) ) ;
#7193 = CARTESIAN_POINT ( 'NONE',  ( 0.000000000000000000, 3.755786496842902015E-16, 3.500000000000000000 ) ) ;
#7194 = CARTESIAN_POINT ( 'NONE',  ( 231.0999999999999375, -34.96874999877096002, 97.40192378864668399 ) ) ;
#7195 = CARTESIAN_POINT ( 'NONE',  ( 82.39999999999999147, -33.51562499938548001, -96.81714838363319586 ) ) ;
#7196 = CARTESIAN_POINT ( 'NONE',  ( -82.39999999999999147, -30.36562499938549209, -103.1828516163667899 ) ) ;
#7197 = VERTEX_POINT ( 'NONE', #9565 ) ;
#7198 = CARTESIAN_POINT ( 'NONE',  ( 83.90000000000000568, -32.11874999877097281, 97.40192378864668399 ) ) ;
#7199 = CARTESIAN_POINT ( 'NONE',  ( 229.8435696437499303, -34.75312499938547717, 99.99999999999998579 ) ) ;
#7200 = CARTESIAN_POINT ( 'NONE',  ( 229.8435696437499303, -34.30312499938548143, -50.00000000000011369 ) ) ;
#7201 = DIRECTION ( 'NONE',  ( 0.000000000000000000, 0.000000000000000000, -1.000000000000000000 ) ) ;
#7202 = ORIENTED_EDGE ( 'NONE', *, *, #10300, .F. ) ;
#7203 = CARTESIAN_POINT ( 'NONE',  ( -85.15643035624999868, -33.70312499938548711, -98.40857419181659793 ) ) ;
#7204 = PLANE ( 'NONE',  #3180 ) ;
#7205 = EDGE_CURVE ( 'NONE', #6188, #5794, #10689, .T. ) ;
#7206 = ORIENTED_EDGE ( 'NONE', *, *, #19047, .F. ) ;
#7207 = CARTESIAN_POINT ( 'NONE',  ( -79.39999999999999147, -30.18750000000000355, 98.26794919243110371 ) ) ;
#7208 = CARTESIAN_POINT ( 'NONE',  ( -82.39999999999999147, -31.49062499938548854, -96.81714838363319586 ) ) ;
#7209 = CARTESIAN_POINT ( 'NONE',  ( 231.0999999999999375, -33.61874999877096570, -52.59807621135342970 ) ) ;
#7210 = CARTESIAN_POINT ( 'NONE',  ( -85.40000000000000568, -31.78124999877096712, -101.7320508075688679 ) ) ;
#7211 = CARTESIAN_POINT ( 'NONE',  ( 232.5999999999999375, -32.39062499938548001, 103.1828516163667899 ) ) ;
#7212 = CARTESIAN_POINT ( 'NONE',  ( -82.39999999999999147, -34.33124999877097139, 103.4641016151377499 ) ) ;
#7213 = CARTESIAN_POINT ( 'NONE',  ( -85.40000000000000568, -35.30624999877096570, 101.7320508075688679 ) ) ;
#7214 = CARTESIAN_POINT ( 'NONE',  ( -82.39999999999999147, -32.05312499938548854, -103.1828516163667899 ) ) ;
#7215 = CARTESIAN_POINT ( 'NONE',  ( -4.203833317240879275, -1.627343821129593859, -3.597273115243890818 ) ) ;
#7216 = CARTESIAN_POINT ( 'NONE',  ( -79.39999999999999147, -34.18124999877097281, -101.7320508075688963 ) ) ;
#7217 = CARTESIAN_POINT ( 'NONE',  ( 79.39999999999999147, -31.96874999877096712, -99.99999999999998579 ) ) ;
#7218 = CARTESIAN_POINT ( 'NONE',  ( 229.5999999999999375, -31.76249999999999218, 101.7320508075688679 ) ) ;
#7219 = EDGE_CURVE ( 'NONE', #5564, #17054, #3859, .T. ) ;
#7220 = ORIENTED_EDGE ( 'NONE', *, *, #1234, .T. ) ;
#7221 = CARTESIAN_POINT ( 'NONE',  ( 85.15643035625001289, -34.15312499938548285, -101.5914258081833879 ) ) ;
#7222 = CARTESIAN_POINT ( 'NONE',  ( 235.5999999999999375, -31.96874999877096002, 99.99999999999998579 ) ) ;
#7223 = CARTESIAN_POINT ( 'NONE',  ( 234.0999999999999375, -34.14374999877096428, -52.59807621135342970 ) ) ;
#7224 = EDGE_CURVE ( 'NONE', #5172, #5491, #19041, .T. ) ;
#7225 = CARTESIAN_POINT ( 'NONE',  ( -83.77821517812500929, -32.31562499938548427, 102.3871387122750889 ) ) ;
#7226 = EDGE_LOOP ( 'NONE', ( #3886, #5660, #2633, #7202, #5509 ) ) ;
#7227 = ORIENTED_EDGE ( 'NONE', *, *, #5561, .F. ) ;
#7228 = CARTESIAN_POINT ( 'NONE',  ( 110.0000000000000000, 5.199999999999976197, -150.0000000000000000 ) ) ;
#7229 = CARTESIAN_POINT ( 'NONE',  ( -80.52691934816502339, -34.99999999999999289, -97.94626448418668474 ) ) ;
#7230 = DIRECTION ( 'NONE',  ( 1.735459783503185124E-31, 0.000000000000000000, 1.000000000000000000 ) ) ;
#7231 = VERTEX_POINT ( 'NONE', #14153 ) ;
#7232 = CARTESIAN_POINT ( 'NONE',  ( 0.000000000000000000, 0.000000000000000000, -5.000000000000000000 ) ) ;
#7233 = DIRECTION ( 'NONE',  ( -0.000000000000000000, -0.000000000000000000, -1.000000000000000000 ) ) ;
#7234 = CARTESIAN_POINT ( 'NONE',  ( 82.15584532983331201, -31.99999999999999289, -102.8696726379688329 ) ) ;
#7235 = CIRCLE ( 'NONE', #16612, 2.199999999999993516 ) ;
#7236 =( BOUNDED_CURVE ( )  B_SPLINE_CURVE ( 2, ( #10194, #11368, #16157, #2768, #8724, #14677, #13215, #19186, #5802 ),
 .UNSPECIFIED., .F., .F. ) 
 B_SPLINE_CURVE_WITH_KNOTS ( ( 3, 2, 2, 2, 3 ),
 ( 0.7291666666666668517, 0.7361111111111111605, 0.7500000000000000000, 0.7638888888888888395, 0.7708333333333332593 ),
 .UNSPECIFIED. ) 
 CURVE ( )  GEOMETRIC_REPRESENTATION_ITEM ( )  RATIONAL_B_SPLINE_CURVE ( ( 0.9330127018922194093, 0.9330127018922209636, 1.000000000000000000, 0.8660254037844387076, 1.000000000000000000, 0.8660254037844387076, 1.000000000000000000, 0.9330127018922198534, 0.9330127018922192983 ) ) 
 REPRESENTATION_ITEM ( '' )  );
#7237 = CARTESIAN_POINT ( 'NONE',  ( -83.77821517812500929, -31.07812499938548711, 102.3871387122750889 ) ) ;
#7238 = CARTESIAN_POINT ( 'NONE',  ( -83.90000000000000568, -31.72500000000000142, 102.5980762113533018 ) ) ;
#7239 = EDGE_CURVE ( 'NONE', #17788, #4300, #9861, .T. ) ;
#7240 = CARTESIAN_POINT ( 'NONE',  ( 234.5119179762160684, -35.00000000000002132, -52.19519922920401456 ) ) ;
#7241 = FACE_OUTER_BOUND ( 'NONE', #7439, .T. ) ;
#7242 = CARTESIAN_POINT ( 'NONE',  ( 85.00132729414795563, -34.99999999999999289, 98.78874432549832818 ) ) ;
#7243 = CARTESIAN_POINT ( 'NONE',  ( 231.2217848218749339, -30.66562499938547859, 97.61286128772489690 ) ) ;
#7244 = ORIENTED_EDGE ( 'NONE', *, *, #8793, .T. ) ;
#7245 = CARTESIAN_POINT ( 'NONE',  ( -79.64356964375001269, -30.77812499938548285, -101.5914258081833879 ) ) ;
#7246 = CARTESIAN_POINT ( 'NONE',  ( 235.5999999999999375, -33.31874999877096144, -50.00000000000011369 ) ) ;
#7247 = VECTOR ( 'NONE', #13607, 1000.000000000000000 ) ;
#7248 = CARTESIAN_POINT ( 'NONE',  ( 233.4038475772933054, -33.73259618943232852, 96.99999999999998579 ) ) ;
#7249 = CARTESIAN_POINT ( 'NONE',  ( 3.333333333333332593, 2.694301256218250007, -3.300726591567078483 ) ) ;
#7250 = CARTESIAN_POINT ( 'NONE',  ( -85.15643035624999868, -30.55312499938548854, 101.5914258081833879 ) ) ;
#7251 = CARTESIAN_POINT ( 'NONE',  ( -83.90000000000000568, -33.97500000000000853, 102.5980762113533018 ) ) ;
#7252 = EDGE_CURVE ( 'NONE', #11363, #3019, #9961, .T. ) ;
#7253 = CARTESIAN_POINT ( 'NONE',  ( 231.2217848218749339, -33.81562499938547717, -52.38713871227520968 ) ) ;
#7254 = VERTEX_POINT ( 'NONE', #2520 ) ;
#7255 = ORIENTED_EDGE ( 'NONE', *, *, #1016, .F. ) ;
#7256 = CARTESIAN_POINT ( 'NONE',  ( -85.40000000000000568, -31.76249999999999929, 101.7320508075688821 ) ) ;
#7257 = CARTESIAN_POINT ( 'NONE',  ( -80.90000000000000568, -31.94999999999999929, 97.40192378864668399 ) ) ;
#7258 = CARTESIAN_POINT ( 'NONE',  ( 82.40000000000000568, -32.30624999877097281, -97.00000000000000000 ) ) ;
#7259 = CARTESIAN_POINT ( 'NONE',  ( 80.90000000000000568, -30.15000000000000213, 102.5980762113533018 ) ) ;
#7260 = PLANE ( 'NONE',  #14916 ) ;
#7262 = AXIS2_PLACEMENT_3D ( 'NONE', #4993, #10936, #15431 ) ;
#7261 = CARTESIAN_POINT ( 'NONE',  ( 233.9782151781249411, -31.79062499938548214, 102.3871387122750889 ) ) ;
#7263 = CARTESIAN_POINT ( 'NONE',  ( 231.2217848218749339, -33.36562499938548143, -52.38713871227520968 ) ) ;
#7264 = CARTESIAN_POINT ( 'NONE',  ( 110.0000000000000000, 10.19999999999997620, -130.0000000000000000 ) ) ;
#7265 = CARTESIAN_POINT ( 'NONE',  ( 79.64356964375001269, -34.00312499938549138, 98.40857419181659793 ) ) ;
#7266 = CARTESIAN_POINT ( 'NONE',  ( 81.02178482187500208, -32.54062499938548569, -97.61286128772489690 ) ) ;
#7267 = CARTESIAN_POINT ( 'NONE',  ( 231.0999999999999375, -30.82499999999999574, -47.40192378864679768 ) ) ;
#7268 = CARTESIAN_POINT ( 'NONE',  ( 232.5999999999999659, -32.58749999999999858, 103.0000000000000000 ) ) ;
#7269 = CARTESIAN_POINT ( 'NONE',  ( 4.180345136606690382, -2.085999704580137060, -3.570468642550115757 ) ) ;
#7270 = ORIENTED_EDGE ( 'NONE', *, *, #3489, .T. ) ;
#7271 = CARTESIAN_POINT ( 'NONE',  ( 79.64356964374999848, -34.07812499938548711, 99.99999999999998579 ) ) ;
#7272 = CARTESIAN_POINT ( 'NONE',  ( 232.5999999999999375, -33.71249999999999147, 96.99999999999998579 ) ) ;
#7273 = CARTESIAN_POINT ( 'NONE',  ( -80.90000000000000568, -34.80000000000000426, 102.5980762113533018 ) ) ;
#7274 = VECTOR ( 'NONE', #6529, 1000.000000000000000 ) ;
#7275 = CARTESIAN_POINT ( 'NONE',  ( -81.02178482187500208, -33.59062499938548285, 102.3871387122750889 ) ) ;
#7276 = ORIENTED_EDGE ( 'NONE', *, *, #17283, .F. ) ;
#7277 = CARTESIAN_POINT ( 'NONE',  ( -83.65502553130849606, -35.00000000000002842, 102.4885329066896702 ) ) ;
#7278 = CARTESIAN_POINT ( 'NONE',  ( 233.9782151781249411, -32.09062499938547575, 97.61286128772489690 ) ) ;
#7279 = DIRECTION ( 'NONE',  ( -0.000000000000000000, -0.000000000000000000, 1.000000000000000000 ) ) ;
#7280 =( BOUNDED_CURVE ( )  B_SPLINE_CURVE ( 2, ( #9002, #17805, #5981, #8807, #7535, #2945, #14962, #8898, #14764 ),
 .UNSPECIFIED., .F., .F. ) 
 B_SPLINE_CURVE_WITH_KNOTS ( ( 3, 2, 2, 2, 3 ),
 ( 0.6458333333333332593, 0.6527777777777777901, 0.6666666666666666297, 0.6805555555555555802, 0.6875000000000000000 ),
 .UNSPECIFIED. ) 
 CURVE ( )  GEOMETRIC_REPRESENTATION_ITEM ( )  RATIONAL_B_SPLINE_CURVE ( ( 0.9330127018922192983, 0.9330127018922187432, 1.000000000000000000, 0.8660254037844387076, 1.000000000000000000, 0.8660254037844387076, 1.000000000000000000, 0.9330127018922194093, 0.9330127018922194093 ) ) 
 REPRESENTATION_ITEM ( '' )  );
#7281 = CARTESIAN_POINT ( 'NONE',  ( -80.90000000000000568, -32.54606250001229739, 102.5980762113533018 ) ) ;
#7282 = CARTESIAN_POINT ( 'NONE',  ( 82.40000000000001990, -34.16250000000000853, -97.00000000000000000 ) ) ;
#7283 = CARTESIAN_POINT ( 'NONE',  ( -80.08630547029558500, -32.02340763552836478, 102.1282894555903198 ) ) ;
#7284 = CARTESIAN_POINT ( 'NONE',  ( -81.02178482187500208, -32.69062499938548427, 102.3871387122750889 ) ) ;
#7285 = LINE ( 'NONE', #14412, #18301 ) ;
#7286 = CARTESIAN_POINT ( 'NONE',  ( 83.77821517812500929, -33.77812499938548285, 97.61286128772489690 ) ) ;
#7287 = LINE ( 'NONE', #13530, #4587 ) ;
#7288 = CARTESIAN_POINT ( 'NONE',  ( 232.5999999999999091, -33.03749999999998721, -47.00000000000011369 ) ) ;
#7289 = CARTESIAN_POINT ( 'NONE',  ( 85.15643035625001289, -33.40312499938548285, -99.99999999999998579 ) ) ;
#7290 = CARTESIAN_POINT ( 'NONE',  ( -82.39999999999999147, -32.16562499938549280, -103.1828516163667899 ) ) ;
#7291 = EDGE_LOOP ( 'NONE', ( #3448, #7494, #8733, #10380 ) ) ;
#7292 = CARTESIAN_POINT ( 'NONE',  ( 80.90000000000000568, -32.04374999877096997, 97.40192378864668399 ) ) ;
#7293 = ITEM_DEFINED_TRANSFORMATION ( 'NONE', 'NONE', #13912,  #10540 ) ;
#7294 = CARTESIAN_POINT ( 'NONE',  ( 85.40000000000000568, -34.48124999877096997, 101.7320508075688821 ) ) ;
#7295 = CARTESIAN_POINT ( 'NONE',  ( 80.80006050682045782, -31.99999999999997868, 102.4537706361795131 ) ) ;
#7296 = ORIENTED_EDGE ( 'NONE', *, *, #12684, .F. ) ;
#7297 = CARTESIAN_POINT ( 'NONE',  ( -81.02178482187500208, -34.49062499938548854, -97.61286128772489690 ) ) ;
#7298 = CARTESIAN_POINT ( 'NONE',  ( 3.999999999999998224, 2.472263674411418588, -3.687027874309861897 ) ) ;
#7299 = ORIENTED_EDGE ( 'NONE', *, *, #4450, .F. ) ;
#7300 = CARTESIAN_POINT ( 'NONE',  ( -80.90000000000000568, -30.30000000000000426, 102.5980762113533018 ) ) ;
#7301 = CARTESIAN_POINT ( 'NONE',  ( -79.64356964374999848, -34.52812499938548285, -99.99999999999998579 ) ) ;
#7302 = DIRECTION ( 'NONE',  ( 6.938893903907244155E-16, 0.5000000000000009992, 0.8660254037844380415 ) ) ;
#7303 = CARTESIAN_POINT ( 'NONE',  ( -79.39999999999999147, -30.61874999877096926, -99.99999999999998579 ) ) ;
#7304 = CARTESIAN_POINT ( 'NONE',  ( 229.8435696437499871, -32.01562499938548001, 101.5914258081833879 ) ) ;
#7305 = CARTESIAN_POINT ( 'NONE',  ( -83.90000000000000568, -33.91874999877096997, 102.5980762113533018 ) ) ;
#7306 = CARTESIAN_POINT ( 'NONE',  ( -79.64356964374999848, -34.52812499938548285, 99.99999999999998579 ) ) ;
#7307 = CARTESIAN_POINT ( 'NONE',  ( -85.40000000000000568, -33.50624999877096855, 101.7320508075688821 ) ) ;
#7308 = EDGE_CURVE ( 'NONE', #15492, #1391, #13492, .T. ) ;
#7309 = LINE ( 'NONE', #13553, #1190 ) ;
#7310 =( BOUNDED_CURVE ( )  B_SPLINE_CURVE ( 2, ( #10049, #16007, #6135, #15111, #3189, #17957, #3093, #13829, #4771 ),
 .UNSPECIFIED., .F., .F. ) 
 B_SPLINE_CURVE_WITH_KNOTS ( ( 3, 2, 2, 2, 3 ),
 ( 0.8125000000000001110, 0.8194444444444444198, 0.8333333333333333703, 0.8472222222222222099, 0.8530683953269213582 ),
 .UNSPECIFIED. ) 
 CURVE ( )  GEOMETRIC_REPRESENTATION_ITEM ( )  RATIONAL_B_SPLINE_CURVE ( ( 0.9330127018922194093, 0.9330127018922204085, 1.000000000000000000, 0.8660254037844387076, 1.000000000000000000, 0.8660254037844387076, 1.000000000000000000, 0.9436068149601996025, 0.9346881722405915305 ) ) 
 REPRESENTATION_ITEM ( '' )  );
#7311 = CARTESIAN_POINT ( 'NONE',  ( -82.40000000000001990, -33.93750000000000711, -97.00000000000000000 ) ) ;
#7312 = CARTESIAN_POINT ( 'NONE',  ( 79.39999999999999147, -31.06874999877096855, -99.99999999999998579 ) ) ;
#7313 = CARTESIAN_POINT ( 'NONE',  ( 235.5999999999999375, -32.92499999999999716, 99.99999999999998579 ) ) ;
#7314 = EDGE_CURVE ( 'NONE', #12396, #16985, #8260, .T. ) ;
#7315 = EDGE_CURVE ( 'NONE', #15349, #16451, #9397, .T. ) ;
#7316 = VERTEX_POINT ( 'NONE', #8477 ) ;
#7317 = CARTESIAN_POINT ( 'NONE',  ( 85.15643035625001289, -34.67812499938548143, -98.40857419181659793 ) ) ;
#7318 = SURFACE_SIDE_STYLE ('',( #19246 ) ) ;
#7319 = CARTESIAN_POINT ( 'NONE',  ( 229.5999999999999375, -32.23124999877096286, 98.26794919243111792 ) ) ;
#7320 = CARTESIAN_POINT ( 'NONE',  ( 229.5999999999999375, -34.44374999877096144, -50.00000000000011369 ) ) ;
#7321 = CARTESIAN_POINT ( 'NONE',  ( -85.15643035625001289, -32.80312499938548854, 101.5914258081833879 ) ) ;
#7322 = ORIENTED_EDGE ( 'NONE', *, *, #7470, .T. ) ;
#7323 = VERTEX_POINT ( 'NONE', #17576 ) ;
#7324 = CARTESIAN_POINT ( 'NONE',  ( -83.52022063339109081, -31.99999999999999289, 97.42682425340038321 ) ) ;
#7325 = FACE_OUTER_BOUND ( 'NONE', #19153, .T. ) ;
#7326 = CARTESIAN_POINT ( 'NONE',  ( 235.5999999999999943, -34.23749999999999716, -51.73205080756900287 ) ) ;
#7327 = ORIENTED_EDGE ( 'NONE', *, *, #2039, .T. ) ;
#7328 = LINE ( 'NONE', #4596, #5480 ) ;
#7329 = CARTESIAN_POINT ( 'NONE',  ( 84.70388354820681798, -35.00002705695767702, 101.9214814096700934 ) ) ;
#7330 = DIRECTION ( 'NONE',  ( -0.000000000000000000, -1.000000000000000000, -0.000000000000000000 ) ) ;
#7331 = ADVANCED_FACE ( 'NONE', ( #12789 ), #15393, .F. ) ;
#7332 = CARTESIAN_POINT ( 'NONE',  ( -83.77821517812500929, -33.77812499938548285, 102.3871387122750889 ) ) ;
#7333 = CARTESIAN_POINT ( 'NONE',  ( -85.40000000000000568, -33.11250000000000426, 101.7320508075688679 ) ) ;
#7334 = EDGE_CURVE ( 'NONE', #13533, #13276, #14823, .T. ) ;
#7335 = CARTESIAN_POINT ( 'NONE',  ( -79.39999999999999147, -32.45624999877097139, 101.7320508075688537 ) ) ;
#7336 = FACE_OUTER_BOUND ( 'NONE', #19147, .T. ) ;
#7337 = CARTESIAN_POINT ( 'NONE',  ( -84.69814089128830403, -35.06584585096306483, 98.07164618293482761 ) ) ;
#7338 = CYLINDRICAL_SURFACE ( 'NONE', #12732, 3.000000000000002665 ) ;
#7339 = CARTESIAN_POINT ( 'NONE',  ( 232.5999999999999375, -30.70312499938548001, 96.81714838363319586 ) ) ;
#7340 = ORIENTED_EDGE ( 'NONE', *, *, #15097, .F. ) ;
#7341 = CARTESIAN_POINT ( 'NONE',  ( 0.000000000000000000, 0.000000000000000000, 0.000000000000000000 ) ) ;
#7342 = CARTESIAN_POINT ( 'NONE',  ( -81.02178482187500208, -34.90312499938548285, -102.3871387122750889 ) ) ;
#7343 = CARTESIAN_POINT ( 'NONE',  ( 232.5999999999999375, -32.36249999999999716, -53.00000000000011369 ) ) ;
#7344 = AXIS2_PLACEMENT_3D ( 'NONE', #10524, #89, #11989 ) ;
#7345 = DIRECTION ( 'NONE',  ( 0.000000000000000000, 0.000000000000000000, 1.000000000000000000 ) ) ;
#7346 = CARTESIAN_POINT ( 'NONE',  ( -83.20384757729335945, -32.73615380933863150, 96.99999999999998579 ) ) ;
#7347 = CARTESIAN_POINT ( 'NONE',  ( -85.15643035625001289, -31.04062499938548569, 99.99999999999998579 ) ) ;
#7348 = PLANE ( 'NONE',  #9734 ) ;
#7349 = CARTESIAN_POINT ( 'NONE',  ( 229.8435696437499871, -32.87812499938547717, -51.59142580818350865 ) ) ;
#7350 =( BOUNDED_CURVE ( )  B_SPLINE_CURVE ( 2, ( #13314, #10102, #1312, #15872, #14779, #16058, #8623, #5709, #5521 ),
 .UNSPECIFIED., .F., .F. ) 
 B_SPLINE_CURVE_WITH_KNOTS ( ( 3, 2, 2, 2, 3 ),
 ( 0.4791666666666666297, 0.4861111111111111049, 0.5000000000000000000, 0.5138888888888888395, 0.5208333333333333703 ),
 .UNSPECIFIED. ) 
 CURVE ( )  GEOMETRIC_REPRESENTATION_ITEM ( )  RATIONAL_B_SPLINE_CURVE ( ( 0.9330127018922194093, 0.9330127018922190762, 1.000000000000000000, 0.8660254037844387076, 1.000000000000000000, 0.8660254037844387076, 1.000000000000000000, 0.9330127018922187432, 0.9330127018922192983 ) ) 
 REPRESENTATION_ITEM ( '' )  );
#7351 = ORIENTED_EDGE ( 'NONE', *, *, #217, .F. ) ;
#7352 = ORIENTED_EDGE ( 'NONE', *, *, #11128, .T. ) ;
#7353 = CARTESIAN_POINT ( 'NONE',  ( 0.02993401039713761494, -2.688325911136454138, 2.343682934607770108 ) ) ;
#7354 = CARTESIAN_POINT ( 'NONE',  ( -80.90000000000000568, -30.60000000000000142, 97.40192378864668399 ) ) ;
#7355 = CARTESIAN_POINT ( 'NONE',  ( -80.90000000000000568, -30.99374999877096926, 97.40192378864668399 ) ) ;
#7356 = CARTESIAN_POINT ( 'NONE',  ( 83.77821517812500929, -34.56562499938548427, 97.61286128772489690 ) ) ;
#7357 = CYLINDRICAL_SURFACE ( 'NONE', #9621, 3.000000000000002665 ) ;
#7358 = CARTESIAN_POINT ( 'NONE',  ( 235.3564303562499447, -31.71562499938547575, 99.99999999999998579 ) ) ;
#7359 = AXIS2_PLACEMENT_3D ( 'NONE', #12469, #12377, #666 ) ;
#7360 = CARTESIAN_POINT ( 'NONE',  ( 229.8435696437499587, -34.22812499938547859, -51.59142580818350154 ) ) ;
#7361 = CARTESIAN_POINT ( 'NONE',  ( 79.64356964374999848, -34.41562499938548569, 99.99999999999998579 ) ) ;
#7362 = CARTESIAN_POINT ( 'NONE',  ( 85.15643035624999868, -31.07812499938548356, -98.40857419181659793 ) ) ;
#7363 = CARTESIAN_POINT ( 'NONE',  ( 229.8435696437499871, -34.67812499938547433, -51.59142580818350865 ) ) ;
#7364 = DIRECTION ( 'NONE',  ( 0.000000000000000000, -1.000000000000000000, 0.000000000000000000 ) ) ;
#7365 = CARTESIAN_POINT ( 'NONE',  ( 79.64356964375001269, -32.12812499938548427, -98.40857419181659793 ) ) ;
#7366 =( GEOMETRIC_REPRESENTATION_CONTEXT ( 3 ) GLOBAL_UNCERTAINTY_ASSIGNED_CONTEXT ( ( #8016 ) ) GLOBAL_UNIT_ASSIGNED_CONTEXT ( ( #2342, #6755, #12799 ) ) REPRESENTATION_CONTEXT ( 'NONE', 'WORKASPACE' ) );
#7367 = ORIENTED_EDGE ( 'NONE', *, *, #1723, .F. ) ;
#7368 = LINE ( 'NONE', #7467, #7247 ) ;
#7369 = FACE_OUTER_BOUND ( 'NONE', #2279, .T. ) ;
#7370 = ADVANCED_FACE ( 'NONE', ( #15657 ), #816, .F. ) ;
#7371 = FACE_OUTER_BOUND ( 'NONE', #3481, .T. ) ;
#7372 = CARTESIAN_POINT ( 'NONE',  ( -83.77821517812500929, -33.21562499938548285, 102.3871387122750889 ) ) ;
#7373 = ORIENTED_EDGE ( 'NONE', *, *, #9892, .F. ) ;
#7374 = CARTESIAN_POINT ( 'NONE',  ( -82.39999999999999147, -32.81250000000000000, 97.00000000000000000 ) ) ;
#7375 = CARTESIAN_POINT ( 'NONE',  ( 229.8435696437499587, -32.80312499938548143, 101.5914258081833879 ) ) ;
#7376 = CARTESIAN_POINT ( 'NONE',  ( 5.560781378645573980, 6.809993116116507654E-16, -4.000000000000000000 ) ) ;
#7377 = CARTESIAN_POINT ( 'NONE',  ( -79.39999999999999147, -32.88356250001229597, 98.26794919243110371 ) ) ;
#7378 = DIRECTION ( 'NONE',  ( 0.000000000000000000, 0.000000000000000000, 1.000000000000000000 ) ) ;
#7379 = CARTESIAN_POINT ( 'NONE',  ( 232.6092389720419646, -31.99999999999999289, -47.13047754280724178 ) ) ;
#7380 = CARTESIAN_POINT ( 'NONE',  ( -82.39999999999999147, -31.82812499938548356, 103.1828516163667899 ) ) ;
#7381 = CARTESIAN_POINT ( 'NONE',  ( 235.5999999999999943, -32.06249999999999289, 101.7320508075688537 ) ) ;
#7382 = CARTESIAN_POINT ( 'NONE',  ( 79.64356964375001269, -31.86562499938548143, 98.40857419181659793 ) ) ;
#7383 = LINE ( 'NONE', #13343, #11150 ) ;
#7384 = EDGE_CURVE ( 'NONE', #14449, #15949, #6678, .T. ) ;
#7385 = CARTESIAN_POINT ( 'NONE',  ( 229.5999999999999375, -33.18749999999999289, -51.73205080756898866 ) ) ;
#7386 = CARTESIAN_POINT ( 'NONE',  ( -82.40000000000000568, -30.00000000000000355, 99.99999999999998579 ) ) ;
#7387 = CARTESIAN_POINT ( 'NONE',  ( -83.77821517812500929, -31.22812499938548569, -102.3871387122750889 ) ) ;
#7388 = ORIENTED_EDGE ( 'NONE', *, *, #6504, .T. ) ;
#7389 = CARTESIAN_POINT ( 'NONE',  ( 85.40000000000000568, -35.30624999877096570, 98.26794919243111792 ) ) ;
#7390 = CYLINDRICAL_SURFACE ( 'NONE', #15520, 3.000000000000002665 ) ;
#7391 = CARTESIAN_POINT ( 'NONE',  ( 232.5999999999999375, -29.99999999999999645, 99.99999999999998579 ) ) ;
#7392 = CARTESIAN_POINT ( 'NONE',  ( -83.77821517812500929, -31.67812499938548498, 97.61286128772489690 ) ) ;
#7393 = CARTESIAN_POINT ( 'NONE',  ( 79.39999999999999147, -33.73124999877096997, -98.26794919243110371 ) ) ;
#7394 = ORIENTED_EDGE ( 'NONE', *, *, #10539, .T. ) ;
#7395 = CARTESIAN_POINT ( 'NONE',  ( -83.77821517812500929, -35.01562499938548711, -97.61286128772489690 ) ) ;
#7396 = VECTOR ( 'NONE', #12095, 1000.000000000000000 ) ;
#7397 = CARTESIAN_POINT ( 'NONE',  ( 244.7999999999999545, -29.80000000000000426, -100.0000000000000000 ) ) ;
#7398 = CARTESIAN_POINT ( 'NONE',  ( -83.77821517812500929, -33.02812499938548285, -102.3871387122750889 ) ) ;
#7399 =( BOUNDED_CURVE ( )  B_SPLINE_CURVE ( 2, ( #10732, #9457, #11018, #16695, #2033, #8097, #6636, #13848, #15522 ),
 .UNSPECIFIED., .F., .F. ) 
 B_SPLINE_CURVE_WITH_KNOTS ( ( 3, 2, 2, 2, 3 ),
 ( 0.8541666666666668517, 0.8611111111111111605, 0.8750000000000000000, 0.8888888888888888395, 0.8958333333333332593 ),
 .UNSPECIFIED. ) 
 CURVE ( )  GEOMETRIC_REPRESENTATION_ITEM ( )  RATIONAL_B_SPLINE_CURVE ( ( 0.9330127018922194093, 0.9330127018922209636, 1.000000000000000000, 0.8660254037844387076, 1.000000000000000000, 0.8660254037844387076, 1.000000000000000000, 0.9330127018922198534, 0.9330127018922192983 ) ) 
 REPRESENTATION_ITEM ( '' )  );
#7400 = CARTESIAN_POINT ( 'NONE',  ( 232.5999999999999375, -33.43124999877096570, -47.00000000000011369 ) ) ;
#7401 = CARTESIAN_POINT ( 'NONE',  ( -82.39999999999999147, -30.73124999877096641, -96.53589838486223584 ) ) ;
#7402 = CARTESIAN_POINT ( 'NONE',  ( 229.8435696437499871, -32.91562499938547859, 101.5914258081833879 ) ) ;
#7403 = CARTESIAN_POINT ( 'NONE',  ( -85.40000000000000568, -32.64768749875867826, 99.99999999999998579 ) ) ;
#7404 = CARTESIAN_POINT ( 'NONE',  ( -82.39999999999999147, -32.61562499938548854, 96.81714838363319586 ) ) ;
#7405 = CARTESIAN_POINT ( 'NONE',  ( -82.39999999999999147, -34.07812499938548711, -96.81714838363319586 ) ) ;
#7406 = CARTESIAN_POINT ( 'NONE',  ( 81.02178482187500208, -34.49062499938548854, 97.61286128772489690 ) ) ;
#7407 = DIRECTION ( 'NONE',  ( 0.000000000000000000, 0.000000000000000000, -1.000000000000000000 ) ) ;
#7408 = CARTESIAN_POINT ( 'NONE',  ( 232.5999999999999375, -33.20624999877097139, 97.00000000000000000 ) ) ;
#7409 = CARTESIAN_POINT ( 'NONE',  ( 79.39999999999999147, -34.70624999877097139, -101.7320508075688537 ) ) ;
#7410 = AXIS2_PLACEMENT_3D ( 'NONE', #2643, #2848, #8998 ) ;
#7411 = CARTESIAN_POINT ( 'NONE',  ( 229.5999999999999375, -33.56249999999999289, 101.7320508075688679 ) ) ;
#7412 = ORIENTED_EDGE ( 'NONE', *, *, #6152, .F. ) ;
#7413 = CARTESIAN_POINT ( 'NONE',  ( 79.64356964374999848, -34.41562499938548569, -99.99999999999998579 ) ) ;
#7414 = CARTESIAN_POINT ( 'NONE',  ( 0.000000000000000000, 0.000000000000000000, 0.000000000000000000 ) ) ;
#7415 = CARTESIAN_POINT ( 'NONE',  ( 235.5999999999999943, -34.18124999877096570, 98.26794919243110371 ) ) ;
#7416 = CARTESIAN_POINT ( 'NONE',  ( 234.0999999999999375, -33.24374999877096570, -52.59807621135342970 ) ) ;
#7417 = CARTESIAN_POINT ( 'NONE',  ( -81.02178482187500208, -33.59062499938548285, 102.3871387122750889 ) ) ;
#7418 = AXIS2_PLACEMENT_3D ( 'NONE', #7490, #14710, #16741 ) ;
#7419 = ORIENTED_EDGE ( 'NONE', *, *, #2537, .T. ) ;
#7420 = ORIENTED_EDGE ( 'NONE', *, *, #13639, .T. ) ;
#7421 = FACE_OUTER_BOUND ( 'NONE', #19250, .T. ) ;
#7422 = CARTESIAN_POINT ( 'NONE',  ( -83.20384757729335945, -34.85759618943233562, 102.9999999999999716 ) ) ;
#7423 = DIRECTION ( 'NONE',  ( 1.000000000000000000, 0.000000000000000000, -0.000000000000000000 ) ) ;
#7424 = ORIENTED_EDGE ( 'NONE', *, *, #7927, .F. ) ;
#7425 = CARTESIAN_POINT ( 'NONE',  ( -80.80861089413673426, -34.99999999999999289, 102.2789443502789055 ) ) ;
#7426 = DIRECTION ( 'NONE',  ( 1.000000000000000000, -1.387778780781445478E-15, -2.407412430484046130E-31 ) ) ;
#7427 = AXIS2_PLACEMENT_3D ( 'NONE', #10084, #7053, #7153 ) ;
#7428 = EDGE_CURVE ( 'NONE', #4491, #7737, #17397, .T. ) ;
#7429 = CIRCLE ( 'NONE', #8052, 2.199999999999993516 ) ;
#7430 = CARTESIAN_POINT ( 'NONE',  ( -82.39999999999999147, -34.41562499938547859, 96.81714838363319586 ) ) ;
#7431 = CARTESIAN_POINT ( 'NONE',  ( -79.39999999999999147, -33.37500000000000000, 99.99999999999998579 ) ) ;
#7432 =( BOUNDED_CURVE ( )  B_SPLINE_CURVE ( 2, ( #5969, #7144, #4497, #4206, #8984, #13189, #11724, #10452, #13094 ),
 .UNSPECIFIED., .F., .F. ) 
 B_SPLINE_CURVE_WITH_KNOTS ( ( 3, 2, 2, 2, 3 ),
 ( 0.3541666666666666297, 0.3611111111111111049, 0.3750000000000000000, 0.3888888888888888951, 0.3958333333333334259 ),
 .UNSPECIFIED. ) 
 CURVE ( )  GEOMETRIC_REPRESENTATION_ITEM ( )  RATIONAL_B_SPLINE_CURVE ( ( 0.9330127018922194093, 0.9330127018922190762, 1.000000000000000000, 0.8660254037844387076, 1.000000000000000000, 0.8660254037844387076, 1.000000000000000000, 0.9330127018922185211, 0.9330127018922192983 ) ) 
 REPRESENTATION_ITEM ( '' )  );
#7433 = CARTESIAN_POINT ( 'NONE',  ( -80.90000000000000568, -30.54374999877096997, 97.40192378864668399 ) ) ;
#7434 = DIRECTION ( 'NONE',  ( 1.000000000000000000, 0.000000000000000000, 0.000000000000000000 ) ) ;
#7435 = CONICAL_SURFACE ( 'NONE', #16172, 4.000000000000000000, 0.8911886515913786111 ) ;
#7436 = CARTESIAN_POINT ( 'NONE',  ( 79.60045861139946055, -35.00000000000000711, 100.3117415790902953 ) ) ;
#7437 = CARTESIAN_POINT ( 'NONE',  ( -82.40000000000000568, -30.00000000000000355, 96.99999999999998579 ) ) ;
#7438 = CARTESIAN_POINT ( 'NONE',  ( 229.8435696437499871, -30.55312499938547788, 101.5914258081833879 ) ) ;
#7439 = EDGE_LOOP ( 'NONE', ( #11843, #4230, #4124, #391 ) ) ;
#7440 = CARTESIAN_POINT ( 'NONE',  ( -79.64356964375001269, -33.55312499938548854, -98.40857419181659793 ) ) ;
#7441 = CARTESIAN_POINT ( 'NONE',  ( 246.9999999999999716, -35.00000000000000000, -100.0000000000000000 ) ) ;
#7442 = EDGE_CURVE ( 'NONE', #5820, #18598, #10267, .T. ) ;
#7443 = CARTESIAN_POINT ( 'NONE',  ( 4.000000000000000000, 2.309401076758515803, -0.4999999999999995559 ) ) ;
#7444 = CARTESIAN_POINT ( 'NONE',  ( 4.175813232069147674, -2.061359961916367833, 3.570380186727398542 ) ) ;
#7445 = CARTESIAN_POINT ( 'NONE',  ( -83.77821517812500929, -30.66562499938548569, 97.61286128772489690 ) ) ;
#7446 = CARTESIAN_POINT ( 'NONE',  ( -83.90000000000000568, -34.12500000000000000, 97.40192378864668399 ) ) ;
#7447 = CARTESIAN_POINT ( 'NONE',  ( 235.3564303562499447, -31.71562499938547575, -50.00000000000011369 ) ) ;
#7448 = ORIENTED_EDGE ( 'NONE', *, *, #19056, .T. ) ;
#7449 = ORIENTED_EDGE ( 'NONE', *, *, #7742, .T. ) ;
#7450 = CARTESIAN_POINT ( 'NONE',  ( -84.85729912020876498, -32.00000000000000000, 101.2614033343865856 ) ) ;
#7451 = CARTESIAN_POINT ( 'NONE',  ( -85.40000000000000568, -30.48749999999999716, 98.26794919243111792 ) ) ;
#7452 = EDGE_CURVE ( 'NONE', #8905, #7231, #14084, .T. ) ;
#7453 = CARTESIAN_POINT ( 'NONE',  ( -82.39999999999999147, -31.40624999877097068, 96.53589838486223584 ) ) ;
#7454 = CARTESIAN_POINT ( 'NONE',  ( 79.39999999999999147, -31.12500000000000355, 99.99999999999998579 ) ) ;
#7455 = DIRECTION ( 'NONE',  ( -0.000000000000000000, 1.000000000000000000, 1.224646799147353207E-16 ) ) ;
#7456 = CARTESIAN_POINT ( 'NONE',  ( 233.9782151781249411, -34.34062499938547575, 97.61286128772489690 ) ) ;
#7457 = CARTESIAN_POINT ( 'NONE',  ( 235.3564303562499447, -33.96562499938547575, -50.00000000000011369 ) ) ;
#7458 = CARTESIAN_POINT ( 'NONE',  ( 79.64356964375001269, -34.45312499938548711, 98.40857419181659793 ) ) ;
#7459 = CARTESIAN_POINT ( 'NONE',  ( 85.15643035625001289, -31.49062499938548498, -99.99999999999998579 ) ) ;
#7460 = VERTEX_POINT ( 'NONE', #18694 ) ;
#7461 = CARTESIAN_POINT ( 'NONE',  ( 229.5999999999999375, -30.86249999999999361, -48.26794919243123161 ) ) ;
#7462 = DIRECTION ( 'NONE',  ( 0.000000000000000000, 0.000000000000000000, 1.000000000000000000 ) ) ;
#7463 = CARTESIAN_POINT ( 'NONE',  ( 85.15643035625001289, -34.19062499938548427, -99.99999999999998579 ) ) ;
#7464 =( BOUNDED_CURVE ( )  B_SPLINE_CURVE ( 2, ( #19031, #13067, #2606, #7015, #17280, #3985, #13251, #12968, #10043 ),
 .UNSPECIFIED., .F., .F. ) 
 B_SPLINE_CURVE_WITH_KNOTS ( ( 3, 2, 2, 2, 3 ),
 ( 0.8125000000000000000, 0.8194444444444444198, 0.8333333333333333703, 0.8472222222222222099, 0.8541666666666665186 ),
 .UNSPECIFIED. ) 
 CURVE ( )  GEOMETRIC_REPRESENTATION_ITEM ( )  RATIONAL_B_SPLINE_CURVE ( ( 0.9330127018922194093, 0.9330127018922194093, 1.000000000000000000, 0.8660254037844387076, 1.000000000000000000, 0.8660254037844387076, 1.000000000000000000, 0.9330127018922209636, 0.9330127018922194093 ) ) 
 REPRESENTATION_ITEM ( '' )  );
#7465 = EDGE_CURVE ( 'NONE', #7832, #609, #438, .T. ) ;
#7466 = ORIENTED_EDGE ( 'NONE', *, *, #12259, .F. ) ;
#7467 = CARTESIAN_POINT ( 'NONE',  ( -82.40000000000000568, -30.00000000000000355, 103.0000000000000000 ) ) ;
#7468 = CARTESIAN_POINT ( 'NONE',  ( 82.40000000000000568, -33.93750000000000711, -102.9999999999999858 ) ) ;
#7469 = CARTESIAN_POINT ( 'NONE',  ( 235.3564303562499447, -30.89062499938548001, -51.59142580818350865 ) ) ;
#7470 = EDGE_CURVE ( 'NONE', #9248, #1356, #18398, .T. ) ;
#7471 = CARTESIAN_POINT ( 'NONE',  ( -83.25523545990762386, -35.19352049914630953, 96.73097394877602540 ) ) ;
#7472 = ORIENTED_EDGE ( 'NONE', *, *, #3625, .T. ) ;
#7473 = CARTESIAN_POINT ( 'NONE',  ( -82.40000000000000568, -30.33749999999999858, 102.9999999999999858 ) ) ;
#7474 = CARTESIAN_POINT ( 'NONE',  ( 231.2217848218749339, -34.11562499938548143, 102.3871387122750889 ) ) ;
#7475 = CARTESIAN_POINT ( 'NONE',  ( -79.39999999999999147, -32.43750000000000000, 98.26794919243110371 ) ) ;
#7476 = CARTESIAN_POINT ( 'NONE',  ( -80.90000000000000568, -32.84606250001229455, 97.40192378864668399 ) ) ;
#7477 = CARTESIAN_POINT ( 'NONE',  ( 99.99999999999997158, -29.80000000000000071, 150.0000000000000000 ) ) ;
#7478 = EDGE_CURVE ( 'NONE', #15041, #11485, #9466, .T. ) ;
#7479 = CARTESIAN_POINT ( 'NONE',  ( -81.59615242270663771, -32.51115380933863008, 103.0000000000000000 ) ) ;
#7480 = CARTESIAN_POINT ( 'NONE',  ( -79.64356964375001269, -31.67812499938548143, 98.40857419181659793 ) ) ;
#7481 = CARTESIAN_POINT ( 'NONE',  ( -81.59615242270662350, -33.01740381056767148, 102.9999999999999858 ) ) ;
#7482 = CARTESIAN_POINT ( 'NONE',  ( 81.02178482187500208, -31.45312499938549067, 97.61286128772489690 ) ) ;
#7483 = DIRECTION ( 'NONE',  ( -0.000000000000000000, -1.000000000000000000, -0.000000000000000000 ) ) ;
#7484 = CARTESIAN_POINT ( 'NONE',  ( 232.5999999999999375, -33.26249999999999574, -53.00000000000011369 ) ) ;
#7485 = CARTESIAN_POINT ( 'NONE',  ( -79.64356964374998427, -32.31562499938548427, 101.5914258081833879 ) ) ;
#7486 = CARTESIAN_POINT ( 'NONE',  ( -79.64356964375001269, -30.51562499938548711, -98.40857419181659793 ) ) ;
#7487 = ORIENTED_EDGE ( 'NONE', *, *, #19050, .T. ) ;
#7488 = CARTESIAN_POINT ( 'NONE',  ( 79.39999999999999147, -34.70624999877097139, 98.26794919243113213 ) ) ;
#7489 = FACE_OUTER_BOUND ( 'NONE', #17202, .T. ) ;
#7490 = CARTESIAN_POINT ( 'NONE',  ( 105.1999999999999744, -34.99999999999999289, -100.0000000000000000 ) ) ;
#7491 = CARTESIAN_POINT ( 'NONE',  ( 4.175075985190096262, -2.060370777630129435, -3.568666869285562981 ) ) ;
#7492 = CARTESIAN_POINT ( 'NONE',  ( -79.64356964375001269, -30.96562499938548640, 101.5914258081833879 ) ) ;
#7493 = CARTESIAN_POINT ( 'NONE',  ( 84.28136653320183314, -32.00000000000000711, 102.0145392219077394 ) ) ;
#7494 = ORIENTED_EDGE ( 'NONE', *, *, #10846, .F. ) ;
#7495 = EDGE_CURVE ( 'NONE', #5414, #927, #2073, .T. ) ;
#7496 = CARTESIAN_POINT ( 'NONE',  ( -79.39999999999999147, -30.18750000000000355, -101.7320508075688821 ) ) ;
#7497 = CARTESIAN_POINT ( 'NONE',  ( -1.639008752937070663E-16, -0.3420925509381497198, -3.499999999999999112 ) ) ;
#7498 = CARTESIAN_POINT ( 'NONE',  ( -82.40000000000000568, -30.11250000000000071, 96.99999999999998579 ) ) ;
#7499 = CARTESIAN_POINT ( 'NONE',  ( -82.39999999999999147, -32.61562499938548854, -103.1828516163667899 ) ) ;
#7500 = CARTESIAN_POINT ( 'NONE',  ( 229.5999999999999375, -34.46249999999999147, -48.26794919243123161 ) ) ;
#7501 = CARTESIAN_POINT ( 'NONE',  ( 231.2217848218749339, -32.87812499938547717, 102.3871387122750889 ) ) ;
#7502 = CARTESIAN_POINT ( 'NONE',  ( -85.40000000000000568, -32.16018749875868110, 101.7320508075688679 ) ) ;
#7503 = CARTESIAN_POINT ( 'NONE',  ( -82.39999999999999147, -33.51562499938548001, 96.81714838363319586 ) ) ;
#7504 = CARTESIAN_POINT ( 'NONE',  ( 85.15643035625001289, -33.74062499938548854, 99.99999999999998579 ) ) ;
#7505 = LINE ( 'NONE', #13265, #16468 ) ;
#7506 = CARTESIAN_POINT ( 'NONE',  ( 99.99999999999997158, -5.200000000000008171, 150.0000000000000000 ) ) ;
#7507 = CARTESIAN_POINT ( 'NONE',  ( 82.39999999999999147, -35.23124999877096997, -103.4641016151377499 ) ) ;
#7508 = CARTESIAN_POINT ( 'NONE',  ( 231.0999999999999375, -34.42499999999999716, 102.5980762113533018 ) ) ;
#7509 = ORIENTED_EDGE ( 'NONE', *, *, #7022, .T. ) ;
#7510 = CARTESIAN_POINT ( 'NONE',  ( 229.8435696437499303, -32.95312499938548001, -50.00000000000011369 ) ) ;
#7511 = CARTESIAN_POINT ( 'NONE',  ( 229.8435696437499303, -30.25312499938548072, 99.99999999999998579 ) ) ;
#7512 = CARTESIAN_POINT ( 'NONE',  ( 232.5999999999999375, -33.88124999877096144, -46.53589838486234953 ) ) ;
#7513 = CARTESIAN_POINT ( 'NONE',  ( -83.77821517812500929, -34.26562499938548711, 97.61286128772489690 ) ) ;
#7514 = ORIENTED_EDGE ( 'NONE', *, *, #8745, .T. ) ;
#7515 = ORIENTED_EDGE ( 'NONE', *, *, #8590, .F. ) ;
#7516 = MANIFOLD_SOLID_BREP ( 'M5 Clearance Hole1', #1043 ) ;
#7517 = CARTESIAN_POINT ( 'NONE',  ( 4.132952817037867987, 2.031684012687260399, -3.518979934899751694 ) ) ;
#7518 =( BOUNDED_CURVE ( )  B_SPLINE_CURVE ( 2, ( #9155, #15118, #13649, #7307, #5855, #13264, #11809, #13745, #18156 ),
 .UNSPECIFIED., .F., .F. ) 
 B_SPLINE_CURVE_WITH_KNOTS ( ( 3, 2, 2, 2, 3 ),
 ( 0.5625000000000000000, 0.5694444444444444198, 0.5833333333333333703, 0.5972222222222222099, 0.6041666666666666297 ),
 .UNSPECIFIED. ) 
 CURVE ( )  GEOMETRIC_REPRESENTATION_ITEM ( )  RATIONAL_B_SPLINE_CURVE ( ( 0.9330127018922194093, 0.9330127018922194093, 1.000000000000000000, 0.8660254037844387076, 1.000000000000000000, 0.8660254037844387076, 1.000000000000000000, 0.9330127018922198534, 0.9330127018922192983 ) ) 
 REPRESENTATION_ITEM ( '' )  );
#7519 = FACE_BOUND ( 'NONE', #4692, .T. ) ;
#7520 = CARTESIAN_POINT ( 'NONE',  ( 4.170895651974602991, -4.109780709045316449, 3.824548179337212366E-14 ) ) ;
#7521 = ORIENTED_EDGE ( 'NONE', *, *, #19036, .T. ) ;
#7522 = DIRECTION ( 'NONE',  ( -1.000000000000000000, -0.000000000000000000, -0.000000000000000000 ) ) ;
#7523 = DIRECTION ( 'NONE',  ( 1.387778780781445676E-15, 1.000000000000000000, 0.000000000000000000 ) ) ;
#7524 = CARTESIAN_POINT ( 'NONE',  ( -79.64356964374999848, -33.17812499938548854, 99.99999999999998579 ) ) ;
#7525 = CARTESIAN_POINT ( 'NONE',  ( -80.90000000000000568, -34.80000000000000426, 102.5980762113533018 ) ) ;
#7526 = CARTESIAN_POINT ( 'NONE',  ( -80.90000000000000568, -32.49374999877097281, 102.5980762113533018 ) ) ;
#7527 = LINE ( 'NONE', #6267, #18498 ) ;
#7528 = CARTESIAN_POINT ( 'NONE',  ( -99.99999999999998579, -35.00000000000000000, 150.0000000000000000 ) ) ;
#7529 = CARTESIAN_POINT ( 'NONE',  ( -79.77811200999879304, -35.00000000000000000, -99.14934632385212865 ) ) ;
#7530 = EDGE_CURVE ( 'NONE', #8610, #5766, #12523, .T. ) ;
#7531 = CARTESIAN_POINT ( 'NONE',  ( 235.3564303562499447, -30.85312499938547859, 101.5914258081833879 ) ) ;
#7532 = VERTEX_POINT ( 'NONE', #13195 ) ;
#7533 =( LENGTH_UNIT ( ) NAMED_UNIT ( * ) SI_UNIT ( .MILLI., .METRE. ) );
#7534 = CARTESIAN_POINT ( 'NONE',  ( -79.64356964374999848, -32.61562499938548854, -99.99999999999998579 ) ) ;
#7535 = CARTESIAN_POINT ( 'NONE',  ( -85.40000000000000568, -33.60000000000000142, 99.99999999999998579 ) ) ;
#7536 = CARTESIAN_POINT ( 'NONE',  ( 99.99999999999994316, -29.80000000000000782, 150.0000000000000000 ) ) ;
#7537 = CARTESIAN_POINT ( 'NONE',  ( -85.15643035624999868, -31.52812499938547930, 98.40857419181659793 ) ) ;
#7538 = CARTESIAN_POINT ( 'NONE',  ( 105.1999999999999886, -4.999999999999993783, -103.0000000000000995 ) ) ;
#7539 = UNCERTAINTY_MEASURE_WITH_UNIT (LENGTH_MEASURE( 1.000000000000000082E-05 ), #809, 'distance_accuracy_value', 'NONE');
#7540 = CARTESIAN_POINT ( 'NONE',  ( 232.5999999999999375, -32.05312499938548143, -53.18285161636690361 ) ) ;
#7541 = ORIENTED_EDGE ( 'NONE', *, *, #13926, .F. ) ;
#7542 = ORIENTED_EDGE ( 'NONE', *, *, #11616, .T. ) ;
#7543 = DIRECTION ( 'NONE',  ( 0.000000000000000000, 0.000000000000000000, 1.000000000000000000 ) ) ;
#7544 = CARTESIAN_POINT ( 'NONE',  ( -82.39999999999999147, -31.23750000000000071, 103.4641016151377499 ) ) ;
#7545 = CARTESIAN_POINT ( 'NONE',  ( -85.40000000000000568, -33.09374999877096712, 99.99999999999998579 ) ) ;
#7546 = CARTESIAN_POINT ( 'NONE',  ( 83.90000000000000568, -32.17500000000000426, 97.40192378864668399 ) ) ;
#7547 = CARTESIAN_POINT ( 'NONE',  ( -82.39076102795762324, -32.00000000000001421, -97.13047754280714230 ) ) ;
#7548 = CARTESIAN_POINT ( 'NONE',  ( 229.8435696437499303, -34.64062499938548001, 99.99999999999998579 ) ) ;
#7549 = CARTESIAN_POINT ( 'NONE',  ( 229.8435696437499303, -34.64062499938548001, -50.00000000000011369 ) ) ;
#7550 = LINE ( 'NONE', #18210, #19307 ) ;
#7551 = EDGE_CURVE ( 'NONE', #6725, #9677, #17512, .T. ) ;
#7552 = AXIS2_PLACEMENT_3D ( 'NONE', #1849, #6545, #14148 ) ;
#7553 = AXIS2_PLACEMENT_3D ( 'NONE', #6466, #4816, #7732 ) ;
#7554 = CARTESIAN_POINT ( 'NONE',  ( 79.64356964374999848, -30.81562499938548427, -99.99999999999998579 ) ) ;
#7555 = ORIENTED_EDGE ( 'NONE', *, *, #16104, .F. ) ;
#7556 = CARTESIAN_POINT ( 'NONE',  ( 232.5999999999999375, -34.52812499938548285, -46.81714838363331666 ) ) ;
#7557 = FACE_OUTER_BOUND ( 'NONE', #11603, .T. ) ;
#7558 = CARTESIAN_POINT ( 'NONE',  ( 81.02178482187500208, -34.34062499938548285, -97.61286128772489690 ) ) ;
#7559 = EDGE_CURVE ( 'NONE', #17250, #10662, #7566, .T. ) ;
#7560 = CARTESIAN_POINT ( 'NONE',  ( 82.40000000000000568, -30.00000000000000355, -99.99999999999998579 ) ) ;
#7561 = DIRECTION ( 'NONE',  ( -0.000000000000000000, -1.000000000000000000, -0.000000000000000000 ) ) ;
#7562 = CARTESIAN_POINT ( 'NONE',  ( 235.3564303562499447, -30.92812499938547788, -50.00000000000011369 ) ) ;
#7563 = CARTESIAN_POINT ( 'NONE',  ( -83.90000000000000568, -30.82500000000000284, 102.5980762113533018 ) ) ;
#7564 = ORIENTED_EDGE ( 'NONE', *, *, #17408, .T. ) ;
#7565 = CARTESIAN_POINT ( 'NONE',  ( -84.97511176747894979, -34.99999999999999289, 98.48300226794593470 ) ) ;
#7566 = CIRCLE ( 'NONE', #1329, 3.000000000000002665 ) ;
#7567 = CIRCLE ( 'NONE', #11932, 5.199999999999996625 ) ;
#7568 = CARTESIAN_POINT ( 'NONE',  ( 229.8435696437499587, -34.15312499938547575, 101.5914258081833879 ) ) ;
#7569 = CARTESIAN_POINT ( 'NONE',  ( 81.02178482187500208, -30.44062499938548783, 97.61286128772489690 ) ) ;
#7570 = CARTESIAN_POINT ( 'NONE',  ( -85.40000000000000568, -32.24606250001229313, 99.99999999999998579 ) ) ;
#7571 = EDGE_CURVE ( 'NONE', #5414, #484, #1006, .T. ) ;
#7572 = CARTESIAN_POINT ( 'NONE',  ( -85.40000000000000568, -33.18750000000000000, -101.7320508075688821 ) ) ;
#7573 = CARTESIAN_POINT ( 'NONE',  ( 96.99999999999997158, -5.200000000000003730, 150.0000000000000000 ) ) ;
#7574 = CARTESIAN_POINT ( 'NONE',  ( 230.2961164517930968, -35.00002705695778360, 98.07851859032987818 ) ) ;
#7575 = CARTESIAN_POINT ( 'NONE',  ( 79.64356964375001269, -30.32812499938548711, 101.5914258081833879 ) ) ;
#7576 = EDGE_CURVE ( 'NONE', #14117, #12107, #14113, .T. ) ;
#7577 = FACE_OUTER_BOUND ( 'NONE', #17998, .T. ) ;
#7578 = DIRECTION ( 'NONE',  ( 0.000000000000000000, 0.000000000000000000, -1.000000000000000000 ) ) ;
#7579 = MANIFOLD_SOLID_BREP ( 'EndChamfer', #15382 ) ;
#7580 = DIRECTION ( 'NONE',  ( 0.000000000000000000, 1.000000000000000000, 0.000000000000000000 ) ) ;
#7581 = CARTESIAN_POINT ( 'NONE',  ( -85.15643035624999868, -31.64062499938548356, -101.5914258081833879 ) ) ;
#7582 = AXIS2_PLACEMENT_3D ( 'NONE', #15551, #8224, #9879 ) ;
#7583 = ORIENTED_EDGE ( 'NONE', *, *, #17371, .F. ) ;
#7584 = CARTESIAN_POINT ( 'NONE',  ( 80.90000000000000568, -34.74374999877097281, 97.40192378864668399 ) ) ;
#7585 = CARTESIAN_POINT ( 'NONE',  ( 83.20384757729337366, -34.35134618820330843, 97.00000000000000000 ) ) ;
#7586 = CARTESIAN_POINT ( 'NONE',  ( 4.104070371397481765, -2.023683613428372219, -3.505122836902507366 ) ) ;
#7587 = CARTESIAN_POINT ( 'NONE',  ( -85.15643035624999868, -31.19062499938548783, 98.40857419181659793 ) ) ;
#7588 = CARTESIAN_POINT ( 'NONE',  ( -84.97511176747885031, -35.00000000000002132, -101.5169977320541790 ) ) ;
#7589 = ORIENTED_EDGE ( 'NONE', *, *, #11638, .F. ) ;
#7590 = CARTESIAN_POINT ( 'NONE',  ( -79.39999999999999147, -32.02500000000000568, -99.99999999999998579 ) ) ;
#7591 = CARTESIAN_POINT ( 'NONE',  ( 82.40000000000001990, -32.53124999877097423, 97.00000000000000000 ) ) ;
#7592 = FACE_OUTER_BOUND ( 'NONE', #11787, .T. ) ;
#7593 = CARTESIAN_POINT ( 'NONE',  ( -81.02178482187500208, -32.80312499938548854, -97.61286128772489690 ) ) ;
#7594 = CARTESIAN_POINT ( 'NONE',  ( -84.28136653320150629, -32.00000000000001421, -102.0145392219080378 ) ) ;
#7595 = CARTESIAN_POINT ( 'NONE',  ( 232.5999999999999375, -31.26562499938548356, 96.81714838363319586 ) ) ;
#7596 = CARTESIAN_POINT ( 'NONE',  ( -80.90000000000000568, -32.79768749875867684, 97.40192378864668399 ) ) ;
#7597 = CARTESIAN_POINT ( 'NONE',  ( -83.77821517812500929, -34.22812499938549280, 102.3871387122750889 ) ) ;
#7598 = CARTESIAN_POINT ( 'NONE',  ( -80.90000000000000568, -31.50000000000000000, 97.40192378864668399 ) ) ;
#7599 = CARTESIAN_POINT ( 'NONE',  ( 85.15643035625001289, -34.19062499938548427, 99.99999999999998579 ) ) ;
#7600 = PLANE ( 'NONE',  #10537 ) ;
#7601 = DIRECTION ( 'NONE',  ( -0.000000000000000000, -1.000000000000000000, -0.000000000000000000 ) ) ;
#7602 = EDGE_CURVE ( 'NONE', #14237, #7460, #4028, .T. ) ;
#7603 = CARTESIAN_POINT ( 'NONE',  ( 85.40000000000000568, -35.34374999877096712, -99.99999999999998579 ) ) ;
#7604 = CARTESIAN_POINT ( 'NONE',  ( 229.5999999999999375, -32.66249999999999432, 101.7320508075688679 ) ) ;
#7605 = EDGE_LOOP ( 'NONE', ( #12809, #10134, #14970, #18887 ) ) ;
#7606 = CARTESIAN_POINT ( 'NONE',  ( 233.9782151781249411, -34.00312499938547717, -52.38713871227520968 ) ) ;
#7607 = CARTESIAN_POINT ( 'NONE',  ( 0.000000000000000000, 0.000000000000000000, 0.000000000000000000 ) ) ;
#7608 = CARTESIAN_POINT ( 'NONE',  ( 234.0999999999999375, -34.14374999877096428, 97.40192378864668399 ) ) ;
#7609 = CARTESIAN_POINT ( 'NONE',  ( 235.5999999999999943, -33.35624999877096997, -48.26794919243124582 ) ) ;
#7610 = CARTESIAN_POINT ( 'NONE',  ( -85.15643035625001289, -33.32812499938548711, 98.40857419181659793 ) ) ;
#7611 = ORIENTED_EDGE ( 'NONE', *, *, #5720, .T. ) ;
#7613 = ORIENTED_EDGE ( 'NONE', *, *, #4576, .T. ) ;
#7612 = EDGE_CURVE ( 'NONE', #13878, #11119, #14575, .T. ) ;
#7614 = FACE_OUTER_BOUND ( 'NONE', #11669, .T. ) ;
#7615 = FACE_OUTER_BOUND ( 'NONE', #1283, .T. ) ;
#7616 = CARTESIAN_POINT ( 'NONE',  ( 82.40000000000000568, -33.03750000000000142, 96.99999999999998579 ) ) ;
#7617 = ORIENTED_EDGE ( 'NONE', *, *, #15618, .T. ) ;
#7618 = CARTESIAN_POINT ( 'NONE',  ( -84.51155153715826884, -35.14114847181267720, 98.22820474807231506 ) ) ;
#7619 = CARTESIAN_POINT ( 'NONE',  ( 232.5999999999999375, -29.99999999999999645, -47.00000000000010658 ) ) ;
#7620 = CARTESIAN_POINT ( 'NONE',  ( -81.02178482187500208, -34.00312499938548427, 97.61286128772489690 ) ) ;
#7621 = CARTESIAN_POINT ( 'NONE',  ( -80.90000000000000568, -33.75000000000000000, 97.40192378864668399 ) ) ;
#7622 = CARTESIAN_POINT ( 'NONE',  ( -80.90000000000000568, -30.69374999877097210, 102.5980762113533018 ) ) ;
#7623 = CARTESIAN_POINT ( 'NONE',  ( 231.0999999999999375, -33.67499999999999716, 97.40192378864668399 ) ) ;
#7624 = CARTESIAN_POINT ( 'NONE',  ( -82.40000000000000568, -30.56250000000001066, 96.99999999999998579 ) ) ;
#7625 = FACE_BOUND ( 'NONE', #986, .T. ) ;
#7626 = CARTESIAN_POINT ( 'NONE',  ( -82.65333140691201663, -34.99995246259153703, -102.9892844631211943 ) ) ;
#7627 = CARTESIAN_POINT ( 'NONE',  ( 231.2217848218749339, -31.86562499938547788, 102.3871387122750889 ) ) ;
#7628 = ORIENTED_EDGE ( 'NONE', *, *, #2560, .F. ) ;
#7629 = CARTESIAN_POINT ( 'NONE',  ( -79.64356964375001269, -34.45312499938548711, -98.40857419181659793 ) ) ;
#7630 = FACE_OUTER_BOUND ( 'NONE', #15315, .T. ) ;
#7631 = SHAPE_REPRESENTATION ( 'grip', ( #10540 ), #12052 ) ;
#7632 = DIRECTION ( 'NONE',  ( 1.000000000000000000, 0.000000000000000000, 0.000000000000000000 ) ) ;
#7633 = CARTESIAN_POINT ( 'NONE',  ( -85.40000000000000568, -32.60624999877096997, 101.7320508075688821 ) ) ;
#7634 = CARTESIAN_POINT ( 'NONE',  ( -82.40000000000001990, -34.61250000000001137, -103.0000000000000000 ) ) ;
#7635 = CARTESIAN_POINT ( 'NONE',  ( 232.5999999999999375, -34.30312499938547433, -53.18285161636690361 ) ) ;
#7636 = ORIENTED_EDGE ( 'NONE', *, *, #6072, .T. ) ;
#7637 = VERTEX_POINT ( 'NONE', #16522 ) ;
#7638 = CARTESIAN_POINT ( 'NONE',  ( -85.40000000000000568, -34.95000000000000284, -99.99999999999998579 ) ) ;
#7639 = CARTESIAN_POINT ( 'NONE',  ( -79.39999999999999147, -31.61250000000000071, 101.7320508075688537 ) ) ;
#7640 = CARTESIAN_POINT ( 'NONE',  ( -79.39999999999999147, -32.45624999877097139, 101.7320508075688537 ) ) ;
#7641 = CARTESIAN_POINT ( 'NONE',  ( 85.40000000000000568, -30.93750000000000355, 101.7320508075688679 ) ) ;
#7642 = CARTESIAN_POINT ( 'NONE',  ( 233.9782151781249411, -32.69062499938547717, 102.3871387122750889 ) ) ;
#7643 = CARTESIAN_POINT ( 'NONE',  ( 233.9782151781249411, -34.04062499938547859, -47.61286128772501769 ) ) ;
#7644 = DIRECTION ( 'NONE',  ( -0.000000000000000000, -1.000000000000000000, -0.000000000000000000 ) ) ;
#7645 = AXIS2_PLACEMENT_3D ( 'NONE', #311, #1944, #6261 ) ;
#7646 = CARTESIAN_POINT ( 'NONE',  ( 81.02178482187500208, -32.99062499938548854, -97.61286128772489690 ) ) ;
#7647 = VERTEX_POINT ( 'NONE', #4408 ) ;
#7648 = CARTESIAN_POINT ( 'NONE',  ( 229.5999999999999375, -33.11249999999999716, -48.26794919243123161 ) ) ;
#7649 = DIRECTION ( 'NONE',  ( 0.000000000000000000, -0.000000000000000000, 1.000000000000000000 ) ) ;
#7650 = CARTESIAN_POINT ( 'NONE',  ( 83.77821517812500929, -33.36562499938548854, -97.61286128772489690 ) ) ;
#7651 = CARTESIAN_POINT ( 'NONE',  ( 82.40000000000000568, -30.00000000000000355, 99.99999999999998579 ) ) ;
#7652 = CARTESIAN_POINT ( 'NONE',  ( 0.000000000000000000, 0.000000000000000000, -4.000000000000000000 ) ) ;
#7653 = CARTESIAN_POINT ( 'NONE',  ( 235.3564303562499447, -32.76562499938548001, -48.40857419181671162 ) ) ;
#7654 = CARTESIAN_POINT ( 'NONE',  ( -79.64356964374999848, -34.86562499938548143, 99.99999999999998579 ) ) ;
#7655 = ORIENTED_EDGE ( 'NONE', *, *, #3251, .T. ) ;
#7656 = CARTESIAN_POINT ( 'NONE',  ( -80.71939127259462055, -35.00048640298293634, 102.4907710001033507 ) ) ;
#7657 = AXIS2_PLACEMENT_3D ( 'NONE', #7477, #16568, #17837 ) ;
#7658 = CARTESIAN_POINT ( 'NONE',  ( -79.39999999999999147, -34.31250000000000000, 101.7320508075688537 ) ) ;
#7659 = CARTESIAN_POINT ( 'NONE',  ( 85.15643035624999868, -30.55312499938548854, 98.40857419181659793 ) ) ;
#7660 = CARTESIAN_POINT ( 'NONE',  ( -82.39999999999999147, -33.48356250001229739, 103.4641016151377499 ) ) ;
#7661 = EDGE_CURVE ( 'NONE', #10662, #15015, #11306, .T. ) ;
#7662 = ADVANCED_FACE ( 'NONE', ( #12212 ), #8891, .T. ) ;
#7663 = CARTESIAN_POINT ( 'NONE',  ( 1.312671235360372224, 3.860931062424219462, -0.05923475698270440348 ) ) ;
#7664 = CARTESIAN_POINT ( 'NONE',  ( -79.64356964374999848, -32.27812499938548996, 99.99999999999998579 ) ) ;
#7665 = CARTESIAN_POINT ( 'NONE',  ( 231.3449744686888891, -35.00000000000002842, 102.4885329066886470 ) ) ;
#7666 = CARTESIAN_POINT ( 'NONE',  ( 81.02178482187500208, -30.29062499938548569, 102.3871387122750889 ) ) ;
#7667 = CARTESIAN_POINT ( 'NONE',  ( 232.5999999999999375, -29.99999999999999645, 96.99999999999998579 ) ) ;
#7668 = CARTESIAN_POINT ( 'NONE',  ( 232.5999999999999375, -30.25312499938548072, -53.18285161636690361 ) ) ;
#7669 = CARTESIAN_POINT ( 'NONE',  ( 83.77821517812500929, -35.12812499938548427, -102.3871387122750889 ) ) ;
#7670 = CARTESIAN_POINT ( 'NONE',  ( -85.15643035624999868, -34.34062499938548285, -101.5914258081833879 ) ) ;
#7671 = AXIS2_PLACEMENT_3D ( 'NONE', #4308, #16033, #14652 ) ;
#7672 = VERTEX_POINT ( 'NONE', #14756 ) ;
#7673 = CARTESIAN_POINT ( 'NONE',  ( 79.39999999999999147, -35.15624999877096712, 98.26794919243113213 ) ) ;
#7674 = LINE ( 'NONE', #16287, #14569 ) ;
#7675 = EDGE_CURVE ( 'NONE', #15015, #17075, #7527, .T. ) ;
#7676 = CARTESIAN_POINT ( 'NONE',  ( -85.40000000000000568, -33.11250000000000426, 101.7320508075688821 ) ) ;
#7677 = EDGE_CURVE ( 'NONE', #3788, #11929, #9082, .T. ) ;
#7678 = CARTESIAN_POINT ( 'NONE',  ( -79.64356964375001269, -32.31562499938548427, 101.5914258081833879 ) ) ;
#7679 = CARTESIAN_POINT ( 'NONE',  ( 234.0999999999999375, -32.09999999999999432, -47.40192378864679768 ) ) ;
#7680 = EDGE_LOOP ( 'NONE', ( #17686, #3322, #10353, #12158 ) ) ;
#7681 = CARTESIAN_POINT ( 'NONE',  ( -79.39999999999999147, -31.53750000000000497, -101.7320508075688821 ) ) ;
#7682 = AXIS2_PLACEMENT_3D ( 'NONE', #5958, #9164, #1743 ) ;
#7683 = DIRECTION ( 'NONE',  ( 0.000000000000000000, 0.000000000000000000, 1.000000000000000000 ) ) ;
#7684 = LINE ( 'NONE', #9437, #14198 ) ;
#7685 = CARTESIAN_POINT ( 'NONE',  ( -83.77821517812500929, -34.22812499938549280, -97.61286128772489690 ) ) ;
#7686 = CARTESIAN_POINT ( 'NONE',  ( -1.274258131565027874, -3.883108878240886241, -3.220599429844051009 ) ) ;
#7687 = EDGE_CURVE ( 'NONE', #14185, #15086, #6321, .T. ) ;
#7688 = CARTESIAN_POINT ( 'NONE',  ( 229.8435696437499871, -33.36562499938548143, 101.5914258081833879 ) ) ;
#7689 = CARTESIAN_POINT ( 'NONE',  ( -83.90000000000000568, -30.92268749875868039, 97.40192378864668399 ) ) ;
#7690 = ORIENTED_EDGE ( 'NONE', *, *, #15093, .T. ) ;
#7691 = CARTESIAN_POINT ( 'NONE',  ( -79.64356964375001269, -33.66562499938549280, 101.5914258081833879 ) ) ;
#7692 = DIRECTION ( 'NONE',  ( 0.000000000000000000, 0.000000000000000000, -1.000000000000000000 ) ) ;
#7693 = CARTESIAN_POINT ( 'NONE',  ( 82.39999999999999147, -33.40312499938548285, 103.1828516163667899 ) ) ;
#7694 = DIRECTION ( 'NONE',  ( -0.000000000000000000, 0.000000000000000000, -1.000000000000000000 ) ) ;
#7695 = DIRECTION ( 'NONE',  ( -0.000000000000000000, -1.000000000000000000, -0.000000000000000000 ) ) ;
#7696 = B_SPLINE_CURVE_WITH_KNOTS ( 'NONE', 3,
 ( #450, #15377, #5033, #7853, #12058, #9316, #16561, #15280, #1704, #1994, #15180, #10597, #9214, #1895, #3163, #13612, #254, #7951, #10973, #13808, #7656, #6211, #6398, #12159, #18127, #4742, #10688, #16656, #1797, #3258, #7761, #13716, #357, #6304, #12254, #12352, #3838, #11071, #15767, #14291, #928, #18800 ),
 .UNSPECIFIED., .F., .F.,
 ( 4, 2, 2, 2, 2, 2, 2, 2, 2, 2, 2, 2, 2, 2, 2, 2, 2, 2, 2, 2, 4 ),
 ( 0.001272204158893248038, 0.06366052697277245487, 0.1260488497866516511, 0.1884371726005308612, 0.2508254954144100712, 0.3132138182282892536, 0.3444079796352281786, 0.3756021410421671036, 0.4379904638560474517, 0.5003787866699277442, 0.5315729480768661697, 0.5627671094838045951, 0.6251554322976795586, 0.6875437551115545221, 0.7187379165184906160, 0.7499320779254269320, 0.8123204007392985648, 0.8747087235531701976, 0.9059028849601048483, 0.9370970463670397210, 0.9994853691809091334 ),
 .UNSPECIFIED. ) ;
#7697 = CARTESIAN_POINT ( 'NONE',  ( 85.40000000000000568, -33.09374999877096712, -99.99999999999998579 ) ) ;
#7698 = CARTESIAN_POINT ( 'NONE',  ( 231.0999999999999375, -33.67499999999999716, 97.40192378864668399 ) ) ;
#7699 = B_SPLINE_CURVE_WITH_KNOTS ( 'NONE', 3,
 ( #3751, #12264, #11078, #8251 ),
 .UNSPECIFIED., .F., .F.,
 ( 4, 4 ),
 ( 0.000000000000000000, 0.002080789711329271950 ),
 .UNSPECIFIED. ) ;
#7700 = ORIENTED_EDGE ( 'NONE', *, *, #11127, .T. ) ;
#7701 = CARTESIAN_POINT ( 'NONE',  ( 233.9782151781249411, -32.35312499938547859, -47.61286128772501769 ) ) ;
#7702 =( LENGTH_UNIT ( ) NAMED_UNIT ( * ) SI_UNIT ( .MILLI., .METRE. ) );
#7703 = CARTESIAN_POINT ( 'NONE',  ( 231.2217848218749339, -30.62812499938548072, 102.3871387122750889 ) ) ;
#7704 = CARTESIAN_POINT ( 'NONE',  ( 231.2217848218749339, -30.62812499938548072, -47.61286128772501769 ) ) ;
#7705 = AXIS2_PLACEMENT_3D ( 'NONE', #15122, #4, #4482 ) ;
#7706 = CARTESIAN_POINT ( 'NONE',  ( -85.39999999999999147, -34.97364041986484295, 98.90809577818235709 ) ) ;
#7707 = ORIENTED_EDGE ( 'NONE', *, *, #19145, .F. ) ;
#7708 = EDGE_LOOP ( 'NONE', ( #1962, #8290, #10439, #7690 ) ) ;
#7709 = CARTESIAN_POINT ( 'NONE',  ( -85.15643035624999868, -30.17812499938548498, -101.5914258081833879 ) ) ;
#7710 = CARTESIAN_POINT ( 'NONE',  ( 232.5999999999999375, -33.93749999999999289, 103.0000000000000000 ) ) ;
#7711 = ORIENTED_EDGE ( 'NONE', *, *, #8055, .T. ) ;
#7712 = CARTESIAN_POINT ( 'NONE',  ( -82.40000000000000568, -30.00000000000000355, 99.99999999999998579 ) ) ;
#7713 = AXIS2_PLACEMENT_3D ( 'NONE', #15862, #16627, #16433 ) ;
#7714 = CARTESIAN_POINT ( 'NONE',  ( 233.4038475772933339, -32.56740381056765443, 102.9999999999999858 ) ) ;
#7715 = CARTESIAN_POINT ( 'NONE',  ( -82.39999999999999147, -34.86562499938548854, 96.81714838363319586 ) ) ;
#7716 = CARTESIAN_POINT ( 'NONE',  ( -80.90000000000000568, -34.64999999999999858, 97.40192378864668399 ) ) ;
#7717 = CARTESIAN_POINT ( 'NONE',  ( -79.39999999999999147, -31.48124999877097352, 98.26794919243110371 ) ) ;
#7718 = CARTESIAN_POINT ( 'NONE',  ( 232.5999999999999375, -29.99999999999999645, 99.99999999999998579 ) ) ;
#7719 = MECHANICAL_DESIGN_GEOMETRIC_PRESENTATION_REPRESENTATION (  '', ( #248 ), #2419 ) ;
#7720 = DIRECTION ( 'NONE',  ( 1.000000000000000000, -0.000000000000000000, -0.000000000000000000 ) ) ;
#7721 = ADVANCED_FACE ( 'NONE', ( #5974 ), #17798, .T. ) ;
#7722 = CARTESIAN_POINT ( 'NONE',  ( 79.39999999999999147, -34.68750000000000000, -98.26794919243110371 ) ) ;
#7723 = LINE ( 'NONE', #12314, #14598 ) ;
#7724 = DIRECTION ( 'NONE',  ( -0.000000000000000000, -1.000000000000000000, -0.000000000000000000 ) ) ;
#7725 = CARTESIAN_POINT ( 'NONE',  ( 231.2217848218749339, -32.31562499938547717, 102.3871387122750889 ) ) ;
#7726 = ORIENTED_EDGE ( 'NONE', *, *, #8279, .F. ) ;
#7727 = VECTOR ( 'NONE', #13871, 1000.000000000000000 ) ;
#7728 = CARTESIAN_POINT ( 'NONE',  ( -83.77821517812500929, -33.36562499938548854, -102.3871387122750889 ) ) ;
#7729 = CARTESIAN_POINT ( 'NONE',  ( 4.071447262713888016, 4.041451884327382338, 0.000000000000000000 ) ) ;
#7730 = DIRECTION ( 'NONE',  ( -0.000000000000000000, -0.000000000000000000, 1.000000000000000000 ) ) ;
#7731 = CARTESIAN_POINT ( 'NONE',  ( 4.050480423730737911, -1.376911654797406959, 3.567926555162024282 ) ) ;
#7732 = DIRECTION ( 'NONE',  ( -1.000000000000000000, 0.000000000000000000, 0.000000000000000000 ) ) ;
#7733 = CARTESIAN_POINT ( 'NONE',  ( -82.40000000000000568, -30.00000000000000355, 99.99999999999998579 ) ) ;
#7734 = VECTOR ( 'NONE', #14557, 1000.000000000000000 ) ;
#7735 = VECTOR ( 'NONE', #1426, 1000.000000000000000 ) ;
#7736 = ORIENTED_EDGE ( 'NONE', *, *, #4040, .T. ) ;
#7737 = VERTEX_POINT ( 'NONE', #8800 ) ;
#7738 = CARTESIAN_POINT ( 'NONE',  ( 81.59615242270662350, -34.76115380933863719, 96.99999999999995737 ) ) ;
#7739 = B_SPLINE_CURVE_WITH_KNOTS ( 'NONE', 3,
 ( #7158, #18986, #15860, #3932, #8613, #11358, #5609, #15760, #14564, #17516, #8329, #17323, #4035, #9995, #6878, #11553, #2647, #19077 ),
 .UNSPECIFIED., .F., .F.,
 ( 4, 2, 2, 2, 2, 2, 2, 2, 4 ),
 ( 0.000000000000000000, 0.0007106627595359582506, 0.001421325519071916501, 0.002131988278607874644, 0.002842651038143833003, 0.003553313797679791362, 0.004263976557215749287, 0.004974639316751707646, 0.005685302076287666005 ),
 .UNSPECIFIED. ) ;
#7740 = CARTESIAN_POINT ( 'NONE',  ( 79.39999999999999147, -30.63750000000000284, -98.26794919243110371 ) ) ;
#7741 = CARTESIAN_POINT ( 'NONE',  ( -85.40000000000000568, -33.13124999877096855, 98.26794919243111792 ) ) ;
#7742 = EDGE_CURVE ( 'NONE', #4852, #17012, #12256, .T. ) ;
#7743 = CARTESIAN_POINT ( 'NONE',  ( 85.40000000000000568, -32.70000000000000284, 99.99999999999998579 ) ) ;
#7744 = AXIS2_PLACEMENT_3D ( 'NONE', #1352, #13356, #7201 ) ;
#7745 = CARTESIAN_POINT ( 'NONE',  ( -81.01744233620665625, -32.00000000000001421, -97.41649131116872695 ) ) ;
#7746 = CARTESIAN_POINT ( 'NONE',  ( 233.9782151781249411, -34.79062499938547859, 97.61286128772489690 ) ) ;
#7747 = CARTESIAN_POINT ( 'NONE',  ( 79.64356964374998427, -33.66562499938548569, -101.5914258081833879 ) ) ;
#7748 = FACE_OUTER_BOUND ( 'NONE', #14206, .T. ) ;
#7749 = SHAPE_REPRESENTATION ( 'knife', ( #10540 ), #4929 ) ;
#7750 = AXIS2_PLACEMENT_3D ( 'NONE', #10343, #17967, #8870 ) ;
#7751 = CARTESIAN_POINT ( 'NONE',  ( 79.64356964375001269, -32.57812499938548001, -98.40857419181659793 ) ) ;
#7752 = ORIENTED_EDGE ( 'NONE', *, *, #10666, .F. ) ;
#7753 = CARTESIAN_POINT ( 'NONE',  ( 234.0999999999999375, -33.74999999999999289, -52.59807621135342970 ) ) ;
#7754 = CARTESIAN_POINT ( 'NONE',  ( 83.77821517812500929, -33.21562499938548285, -102.3871387122750889 ) ) ;
#7755 = CARTESIAN_POINT ( 'NONE',  ( 79.64356964374999848, -33.51562499938548711, -99.99999999999998579 ) ) ;
#7756 = DIRECTION ( 'NONE',  ( -1.000000000000000000, 0.000000000000000000, 0.000000000000000000 ) ) ;
#7757 = CARTESIAN_POINT ( 'NONE',  ( -79.64356964374999848, -32.27812499938548996, 99.99999999999998579 ) ) ;
#7758 = CARTESIAN_POINT ( 'NONE',  ( 231.2217848218749339, -32.42812499938548143, -47.61286128772501769 ) ) ;
#7759 = CARTESIAN_POINT ( 'NONE',  ( -83.90000000000000568, -30.37500000000000355, 102.5980762113533018 ) ) ;
#7760 = VERTEX_POINT ( 'NONE', #10649 ) ;
#7761 = CARTESIAN_POINT ( 'NONE',  ( -79.46741390214279477, -35.00116912023187865, 99.34444296685866505 ) ) ;
#7762 = EDGE_CURVE ( 'NONE', #17929, #10812, #6952, .T. ) ;
#7763 = AXIS2_PLACEMENT_3D ( 'NONE', #2597, #15897, #9939 ) ;
#7764 = CARTESIAN_POINT ( 'NONE',  ( 232.5999999999999943, -33.85312499938547859, 96.81714838363319586 ) ) ;
#7765 = CARTESIAN_POINT ( 'NONE',  ( 79.64356964374999848, -30.81562499938548427, 99.99999999999998579 ) ) ;
#7766 = CARTESIAN_POINT ( 'NONE',  ( 235.5999999999999375, -34.72499999999999432, 99.99999999999998579 ) ) ;
#7767 = CARTESIAN_POINT ( 'NONE',  ( -79.64356964374998427, -30.44062499938548783, 98.40857419181659793 ) ) ;
#7768 = CARTESIAN_POINT ( 'NONE',  ( -80.90000000000000568, -32.85000000000000142, 97.40192378864668399 ) ) ;
#7769 = CARTESIAN_POINT ( 'NONE',  ( 85.15643035624999868, -33.89062499938548711, 101.5914258081833879 ) ) ;
#7770 = CARTESIAN_POINT ( 'NONE',  ( 85.15643035625001289, -30.70312499938548711, -99.99999999999998579 ) ) ;
#7771 = CARTESIAN_POINT ( 'NONE',  ( 233.4038475772933339, -32.83259618943232994, -53.00000000000011369 ) ) ;
#7772 = CARTESIAN_POINT ( 'NONE',  ( 85.15643035625001289, -35.20312499938548711, -99.99999999999998579 ) ) ;
#7773 = CARTESIAN_POINT ( 'NONE',  ( -83.77821517812500929, -33.02812499938548285, -102.3871387122750889 ) ) ;
#7774 = B_SPLINE_CURVE_WITH_KNOTS ( 'NONE', 3,
 ( #803, #5394, #5296, #14262, #10949, #5194, #900, #9877 ),
 .UNSPECIFIED., .F., .F.,
 ( 4, 2, 2, 4 ),
 ( 0.000000000000000000, 0.002450665683189820997, 0.003675998524784731495, 0.004901331366379641993 ),
 .UNSPECIFIED. ) ;
#7775 = VERTEX_POINT ( 'NONE', #16329 ) ;
#7776 = CARTESIAN_POINT ( 'NONE',  ( 83.77821517812500929, -30.32812499938548711, 102.3871387122750889 ) ) ;
#7777 = CARTESIAN_POINT ( 'NONE',  ( 105.1999999999999744, -29.80000000000000071, -100.0000000000000000 ) ) ;
#7778 = CARTESIAN_POINT ( 'NONE',  ( 25.60000000000000142, 0.000000000000000000, 2.055000000000000160 ) ) ;
#7779 = CARTESIAN_POINT ( 'NONE',  ( -82.39999999999999147, -30.59062499938548640, 103.1828516163667899 ) ) ;
#7780 = CARTESIAN_POINT ( 'NONE',  ( -0.3198814748697807464, -4.434118497892185040, -0.3507732604232532969 ) ) ;
#7781 = ORIENTED_EDGE ( 'NONE', *, *, #17556, .T. ) ;
#7782 = CARTESIAN_POINT ( 'NONE',  ( -83.90000000000000568, -30.37500000000000355, -97.40192378864668399 ) ) ;
#7783 = CARTESIAN_POINT ( 'NONE',  ( 84.01447415327271528, -35.02670941564510088, -97.25687757881057394 ) ) ;
#7784 = CARTESIAN_POINT ( 'NONE',  ( 79.39999999999999147, -33.80624999877097281, 98.26794919243113213 ) ) ;
#7785 = CARTESIAN_POINT ( 'NONE',  ( -79.64356964375001269, -35.01562499938548711, -98.40857419181659793 ) ) ;
#7786 = DIRECTION ( 'NONE',  ( -1.000000000000000000, 1.387778780781445676E-15, 2.407412430484046130E-31 ) ) ;
#7787 = CARTESIAN_POINT ( 'NONE',  ( 231.2217848218749339, -33.77812499938547575, 102.3871387122750889 ) ) ;
#7788 = CARTESIAN_POINT ( 'NONE',  ( -79.39999999999999147, -32.01018749875868252, 101.7320508075688537 ) ) ;
#7789 = VERTEX_POINT ( 'NONE', #16616 ) ;
#7790 = CARTESIAN_POINT ( 'NONE',  ( 110.2307692307692832, 5.599704032515842478, 42.03205365446332564 ) ) ;
#7791 = CARTESIAN_POINT ( 'NONE',  ( 79.39999999999999147, -32.90624999877096712, -101.7320508075688537 ) ) ;
#7792 = CARTESIAN_POINT ( 'NONE',  ( 82.39999999999999147, -32.50312499938548427, 103.1828516163667899 ) ) ;
#7793 = CARTESIAN_POINT ( 'NONE',  ( 110.0000000000000000, 5.199999999999975309, -145.0000000000000000 ) ) ;
#7794 = CARTESIAN_POINT ( 'NONE',  ( -82.40000000000000568, -30.00000000000000355, -96.99999999999998579 ) ) ;
#7795 = CARTESIAN_POINT ( 'NONE',  ( 82.39999999999999147, -33.88124999877096855, -103.4641016151377499 ) ) ;
#7796 = DIRECTION ( 'NONE',  ( 2.312964634635736745E-15, 1.000000000000000000, 0.000000000000000000 ) ) ;
#7797 = ORIENTED_EDGE ( 'NONE', *, *, #315, .T. ) ;
#7798 = CARTESIAN_POINT ( 'NONE',  ( 233.9782151781249411, -32.65312499938548285, -52.38713871227520968 ) ) ;
#7799 = DIRECTION ( 'NONE',  ( 0.000000000000000000, 0.000000000000000000, 1.000000000000000000 ) ) ;
#7800 = CARTESIAN_POINT ( 'NONE',  ( 229.8435696437499871, -33.44062499938547717, 98.40857419181659793 ) ) ;
#7801 = CARTESIAN_POINT ( 'NONE',  ( 229.8435696437499303, -30.70312499938548001, -50.00000000000011369 ) ) ;
#7802 = ADVANCED_FACE ( 'NONE', ( #7336 ), #11924, .F. ) ;
#7803 = CARTESIAN_POINT ( 'NONE',  ( -81.02178482187500208, -34.79062499938548569, 97.61286128772489690 ) ) ;
#7804 = ORIENTED_EDGE ( 'NONE', *, *, #2775, .T. ) ;
#7805 = ORIENTED_EDGE ( 'NONE', *, *, #6147, .F. ) ;
#7806 = DIRECTION ( 'NONE',  ( 0.000000000000000000, -1.000000000000000000, 0.000000000000000000 ) ) ;
#7807 = CARTESIAN_POINT ( 'NONE',  ( -81.59615242270665192, -33.67634618820330417, -103.0000000000000000 ) ) ;
#7808 = CARTESIAN_POINT ( 'NONE',  ( 4.082498951862920222, -4.041451884327388555, -2.280731272670711599E-17 ) ) ;
#7809 = ORIENTED_EDGE ( 'NONE', *, *, #13883, .T. ) ;
#7810 = CARTESIAN_POINT ( 'NONE',  ( 85.15643035624999868, -32.02817623523065294, 98.94122380911255732 ) ) ;
#7811 = CARTESIAN_POINT ( 'NONE',  ( -79.39999999999999147, -34.18124999877097281, -101.7320508075688821 ) ) ;
#7812 = CARTESIAN_POINT ( 'NONE',  ( -82.40000000000000568, -34.38749999999999574, 102.9999999999999858 ) ) ;
#7813 = CARTESIAN_POINT ( 'NONE',  ( -82.39999999999999147, -34.61250000000000426, 96.53589838486223584 ) ) ;
#7814 = CARTESIAN_POINT ( 'NONE',  ( -83.90000000000000568, -34.81874999877096855, 102.5980762113533018 ) ) ;
#7815 = CARTESIAN_POINT ( 'NONE',  ( -80.90000000000000568, -30.54374999877096997, 97.40192378864668399 ) ) ;
#7816 = ADVANCED_FACE ( 'NONE', ( #3222 ), #9180, .T. ) ;
#7817 = CARTESIAN_POINT ( 'NONE',  ( 117.5000000000000142, 12.69999999999998508, 50.00000000000001421 ) ) ;
#7818 = SURFACE_STYLE_FILL_AREA ( #14955 ) ;
#7819 = FACE_OUTER_BOUND ( 'NONE', #18870, .T. ) ;
#7820 = CARTESIAN_POINT ( 'NONE',  ( 229.8435696437499303, -33.29062499938547148, 99.99999999999998579 ) ) ;
#7821 = ADVANCED_FACE ( 'NONE', ( #1477 ), #1761, .T. ) ;
#7822 = CARTESIAN_POINT ( 'NONE',  ( 229.8435696437499871, -32.80312499938548143, 101.5914258081833879 ) ) ;
#7823 = EDGE_LOOP ( 'NONE', ( #2534, #8098, #18404, #14596 ) ) ;
#7824 = CARTESIAN_POINT ( 'NONE',  ( -83.77821517812500929, -33.81562499938548427, -102.3871387122750889 ) ) ;
#7825 = CARTESIAN_POINT ( 'NONE',  ( 0.3126073911696408136, 2.020725942163688060, 3.500000000000000000 ) ) ;
#7826 = ORIENTED_EDGE ( 'NONE', *, *, #18220, .T. ) ;
#7827 = LINE ( 'NONE', #13782, #8641 ) ;
#7828 = FACE_OUTER_BOUND ( 'NONE', #11916, .T. ) ;
#7829 = CARTESIAN_POINT ( 'NONE',  ( 112.8867513459481984, 10.19999999999995310, 50.00000000000001421 ) ) ;
#7830 = VERTEX_POINT ( 'NONE', #1579 ) ;
#7831 = CARTESIAN_POINT ( 'NONE',  ( 232.5999999999999375, -33.43124999877096570, 102.9999999999999858 ) ) ;
#7832 = VERTEX_POINT ( 'NONE', #13483 ) ;
#7833 = ORIENTED_EDGE ( 'NONE', *, *, #10203, .T. ) ;
#7834 = DIRECTION ( 'NONE',  ( -1.000000000000000000, -0.000000000000000000, -0.000000000000000000 ) ) ;
#7835 = ADVANCED_FACE ( 'NONE', ( #123 ), #6074, .F. ) ;
#7836 = CARTESIAN_POINT ( 'NONE',  ( 79.64356964374999848, -34.86562499938548143, -99.99999999999998579 ) ) ;
#7837 = CARTESIAN_POINT ( 'NONE',  ( -85.40000000000000568, -33.58124999877097139, 98.26794919243111792 ) ) ;
#7838 = CARTESIAN_POINT ( 'NONE',  ( -83.09162395290293546, -32.00000000000001421, -97.24830349208643554 ) ) ;
#7839 = CARTESIAN_POINT ( 'NONE',  ( 235.3564303562499447, -33.47812499938547148, 98.40857419181659793 ) ) ;
#7840 = CARTESIAN_POINT ( 'NONE',  ( 82.39999999999999147, -33.74062499938548854, -103.1828516163667899 ) ) ;
#7841 = CARTESIAN_POINT ( 'NONE',  ( 82.40000000000001990, -33.88124999877096855, -103.0000000000000000 ) ) ;
#7842 = CARTESIAN_POINT ( 'NONE',  ( 79.64356964375001269, -34.45312499938548711, -101.5914258081833879 ) ) ;
#7843 = ORIENTED_EDGE ( 'NONE', *, *, #2474, .T. ) ;
#7844 = CARTESIAN_POINT ( 'NONE',  ( 234.0999999999999375, -31.94999999999999218, -52.59807621135342970 ) ) ;
#7845 = ADVANCED_FACE ( 'NONE', ( #6651 ), #12596, .F. ) ;
#7846 = CARTESIAN_POINT ( 'NONE',  ( -84.01447415327271528, -35.02670941564510088, 97.25687757881057394 ) ) ;
#7847 = CARTESIAN_POINT ( 'NONE',  ( -83.20384757729335945, -30.99240381056766580, 96.99999999999998579 ) ) ;
#7848 = CARTESIAN_POINT ( 'NONE',  ( 229.8435696437499587, -33.44062499938547717, 98.40857419181659793 ) ) ;
#7849 = CARTESIAN_POINT ( 'NONE',  ( -85.15643035625001289, -32.05312499938548854, 99.99999999999998579 ) ) ;
#7850 = CARTESIAN_POINT ( 'NONE',  ( 229.8435696437499871, -33.36562499938548143, -48.40857419181671162 ) ) ;
#7851 = CARTESIAN_POINT ( 'NONE',  ( -83.90000000000000568, -32.32500000000000284, 97.40192378864668399 ) ) ;
#7852 = ORIENTED_EDGE ( 'NONE', *, *, #3186, .T. ) ;
#7853 = CARTESIAN_POINT ( 'NONE',  ( -85.34334167081365763, -34.99814660107585951, 99.32349799501227494 ) ) ;
#7854 = EDGE_CURVE ( 'NONE', #7830, #13276, #3826, .T. ) ;
#7855 = PRODUCT_RELATED_PRODUCT_CATEGORY ( 'part', '', ( #8424 ) ) ;
#7856 = CARTESIAN_POINT ( 'NONE',  ( -79.39999999999999147, -34.63124999877096855, 98.26794919243110371 ) ) ;
#7857 = CARTESIAN_POINT ( 'NONE',  ( 79.64356964375001269, -30.40312499938548285, 98.40857419181659793 ) ) ;
#7858 = VECTOR ( 'NONE', #17186, 1000.000000000000000 ) ;
#7859 = AXIS2_PLACEMENT_3D ( 'NONE', #13092, #2737, #7230 ) ;
#7860 = CARTESIAN_POINT ( 'NONE',  ( 230.2593261479345301, -32.00000000000000000, -51.46660719531470107 ) ) ;
#7861 = CARTESIAN_POINT ( 'NONE',  ( -82.39999999999999147, -31.26562499938549067, 96.81714838363319586 ) ) ;
#7862 = CARTESIAN_POINT ( 'NONE',  ( 84.12306224665906029, -32.00000000000000000, 97.80849716182737552 ) ) ;
#7863 = CARTESIAN_POINT ( 'NONE',  ( 82.39999999999999147, -34.19062499938548427, 96.81714838363319586 ) ) ;
#7864 = CARTESIAN_POINT ( 'NONE',  ( 79.64356964374999848, -30.92812499938548498, -99.99999999999998579 ) ) ;
#7865 = CARTESIAN_POINT ( 'NONE',  ( 232.5999999999999375, -31.15312499938547930, -53.18285161636690361 ) ) ;
#7866 = CARTESIAN_POINT ( 'NONE',  ( -79.64356964374999848, -34.98839802032725288, 100.4359666841262282 ) ) ;
#7867 = CARTESIAN_POINT ( 'NONE',  ( -81.02178482187500208, -34.15312499938548285, -97.61286128772489690 ) ) ;
#7868 = ORIENTED_EDGE ( 'NONE', *, *, #5074, .F. ) ;
#7869 = CARTESIAN_POINT ( 'NONE',  ( 85.15643035624999868, -31.56562499938548427, 98.40857419181659793 ) ) ;
#7870 = AXIS2_PLACEMENT_3D ( 'NONE', #11253, #6382, #13886 ) ;
#7871 =( NAMED_UNIT ( * ) PLANE_ANGLE_UNIT ( ) SI_UNIT ( $, .RADIAN. ) );
#7872 = AXIS2_PLACEMENT_3D ( 'NONE', #8924, #4642, #10591 ) ;
#7873 = CARTESIAN_POINT ( 'NONE',  ( -85.15643035625001289, -35.20312499938548711, 99.99999999999998579 ) ) ;
#7874 = CARTESIAN_POINT ( 'NONE',  ( -1.144235203016679359, -3.958177651039096911, -0.09382832055446428676 ) ) ;
#7875 = ORIENTED_EDGE ( 'NONE', *, *, #338, .F. ) ;
#7876 = CARTESIAN_POINT ( 'NONE',  ( -79.39999999999999147, -30.71250000000000568, -98.26794919243113213 ) ) ;
#7877 = CARTESIAN_POINT ( 'NONE',  ( 80.90000000000000568, -34.64999999999999858, -97.40192378864668399 ) ) ;
#7878 = CARTESIAN_POINT ( 'NONE',  ( 83.90000000000000568, -34.81874999877096855, -102.5980762113533018 ) ) ;
#7879 = CARTESIAN_POINT ( 'NONE',  ( -81.02178482187500208, -34.90312499938548285, -102.3871387122750889 ) ) ;
#7880 = CARTESIAN_POINT ( 'NONE',  ( 112.9999999999999858, -1.568190022283033361E-13, -2.720376046446971763E-29 ) ) ;
#7881 = CARTESIAN_POINT ( 'NONE',  ( 229.8435696437499303, -30.14062499938548001, 99.99999999999998579 ) ) ;
#7882 = CARTESIAN_POINT ( 'NONE',  ( -80.90000000000000568, -33.24768749875867968, 97.40192378864668399 ) ) ;
#7883 = ORIENTED_EDGE ( 'NONE', *, *, #17523, .F. ) ;
#7884 = DIRECTION ( 'NONE',  ( -0.000000000000000000, -1.000000000000000000, -0.000000000000000000 ) ) ;
#7885 = CARTESIAN_POINT ( 'NONE',  ( 85.40000000000000568, -34.50000000000000000, -99.99999999999998579 ) ) ;
#7886 = CARTESIAN_POINT ( 'NONE',  ( 230.0213320530827730, -31.99999999999999289, 99.01001922939823885 ) ) ;
#7887 = CARTESIAN_POINT ( 'NONE',  ( 85.40000000000000568, -34.40624999877096712, -101.7320508075688821 ) ) ;
#7888 = AXIS2_PLACEMENT_3D ( 'NONE', #6359, #15634, #4895 ) ;
#7889 = FACE_OUTER_BOUND ( 'NONE', #3139, .T. ) ;
#7890 = CARTESIAN_POINT ( 'NONE',  ( 79.64356964374999848, -32.27812499938548996, -99.99999999999998579 ) ) ;
#7891 = CARTESIAN_POINT ( 'NONE',  ( 232.5999999999999375, -29.99999999999999645, 99.99999999999998579 ) ) ;
#7892 = ORIENTED_EDGE ( 'NONE', *, *, #64, .T. ) ;
#7893 = CARTESIAN_POINT ( 'NONE',  ( 235.3564303562499447, -32.31562499938547717, -48.40857419181671162 ) ) ;
#7894 = DIRECTION ( 'NONE',  ( 1.000000000000000000, 0.000000000000000000, 0.000000000000000000 ) ) ;
#7895 = CARTESIAN_POINT ( 'NONE',  ( 235.3564303562499447, -32.76562499938548001, 101.5914258081833879 ) ) ;
#7896 = CARTESIAN_POINT ( 'NONE',  ( 235.3564303562499447, -30.92812499938547788, -50.00000000000011369 ) ) ;
#7897 = CARTESIAN_POINT ( 'NONE',  ( -82.39999999999999147, -32.95312499938548711, 96.81714838363319586 ) ) ;
#7898 = VERTEX_POINT ( 'NONE', #9277 ) ;
#7899 = VERTEX_POINT ( 'NONE', #6554 ) ;
#7900 = CARTESIAN_POINT ( 'NONE',  ( 231.7961524227065695, -32.55134618820330417, -47.00000000000011369 ) ) ;
#7901 = CARTESIAN_POINT ( 'NONE',  ( -82.40000000000000568, -30.73124999877097352, 102.9999999999999858 ) ) ;
#7902 = CARTESIAN_POINT ( 'NONE',  ( -82.40000000000000568, -33.93750000000000711, -97.00000000000000000 ) ) ;
#7903 = VERTEX_POINT ( 'NONE', #13771 ) ;
#7904 = CARTESIAN_POINT ( 'NONE',  ( 82.39999999999999147, -32.16562499938548569, 103.1828516163667899 ) ) ;
#7905 = CARTESIAN_POINT ( 'NONE',  ( -83.90000000000000568, -34.06874999877096855, -102.5980762113533018 ) ) ;
#7906 = CARTESIAN_POINT ( 'NONE',  ( -3.679171394226034675, -2.494631558665844739, -0.3503314178412558211 ) ) ;
#7907 = CARTESIAN_POINT ( 'NONE',  ( -79.39999999999999147, -31.96874999877096712, 99.99999999999998579 ) ) ;
#7908 =( BOUNDED_CURVE ( )  B_SPLINE_CURVE ( 2, ( #3739, #9609, #18505, #9407, #827, #15667, #9311, #6686, #12630 ),
 .UNSPECIFIED., .F., .F. ) 
 B_SPLINE_CURVE_WITH_KNOTS ( ( 3, 2, 2, 2, 3 ),
 ( 0.6458333333333332593, 0.6527777777777777901, 0.6666666666666666297, 0.6805555555555555802, 0.6875000000000000000 ),
 .UNSPECIFIED. ) 
 CURVE ( )  GEOMETRIC_REPRESENTATION_ITEM ( )  RATIONAL_B_SPLINE_CURVE ( ( 0.9330127018922192983, 0.9330127018922187432, 1.000000000000000000, 0.8660254037844387076, 1.000000000000000000, 0.8660254037844387076, 1.000000000000000000, 0.9330127018922194093, 0.9330127018922194093 ) ) 
 REPRESENTATION_ITEM ( '' )  );
#7909 = CARTESIAN_POINT ( 'NONE',  ( -83.90000000000000568, -33.46874999877096712, 102.5980762113533018 ) ) ;
#7910 = CARTESIAN_POINT ( 'NONE',  ( -82.39999999999999147, -32.36250000000000426, 96.99999999999997158 ) ) ;
#7911 = EDGE_CURVE ( 'NONE', #14497, #14237, #18278, .T. ) ;
#7912 = EDGE_CURVE ( 'NONE', #10919, #6974, #16257, .T. ) ;
#7913 = CARTESIAN_POINT ( 'NONE',  ( 102.9999999999999858, -5.200000000000008171, -100.0000000000000000 ) ) ;
#7914 = CARTESIAN_POINT ( 'NONE',  ( 231.0999999999999375, -34.81874999877096144, -47.40192378864679768 ) ) ;
#7915 = CARTESIAN_POINT ( 'NONE',  ( 231.1166048115126443, -35.16733441503057378, 97.47959136244114120 ) ) ;
#7916 = ORIENTED_EDGE ( 'NONE', *, *, #11964, .T. ) ;
#7917 = FILL_AREA_STYLE_COLOUR ( '', #8347 ) ;
#7918 = CARTESIAN_POINT ( 'NONE',  ( -81.02178482187500208, -34.79062499938548569, -102.3871387122750889 ) ) ;
#7919 = LINE ( 'NONE', #13868, #3360 ) ;
#7920 = ORIENTED_EDGE ( 'NONE', *, *, #413, .F. ) ;
#7921 = CARTESIAN_POINT ( 'NONE',  ( 244.7999999999999545, -29.80000000000000426, -100.0000000000000000 ) ) ;
#7922 = DIRECTION ( 'NONE',  ( -0.000000000000000000, -1.000000000000000000, -0.000000000000000000 ) ) ;
#7923 = CARTESIAN_POINT ( 'NONE',  ( 83.20384757729335945, -33.05759618943233136, -102.9999999999999858 ) ) ;
#7924 = ORIENTED_EDGE ( 'NONE', *, *, #13883, .F. ) ;
#7925 = CARTESIAN_POINT ( 'NONE',  ( 235.3564303562499447, -34.37812499938547717, -51.59142580818350865 ) ) ;
#7927 = EDGE_CURVE ( 'NONE', #14213, #14240, #17845, .T. ) ;
#7926 = ORIENTED_EDGE ( 'NONE', *, *, #8215, .T. ) ;
#7928 = ORIENTED_EDGE ( 'NONE', *, *, #12453, .F. ) ;
#7929 = CYLINDRICAL_SURFACE ( 'NONE', #12271, 2.500000000000000444 ) ;
#7930 = CARTESIAN_POINT ( 'NONE',  ( 83.90000000000000568, -31.27500000000000568, -102.5980762113533018 ) ) ;
#7931 = LINE ( 'NONE', #12812, #13292 ) ;
#7932 = EDGE_CURVE ( 'NONE', #7081, #11136, #4794, .T. ) ;
#7933 = CARTESIAN_POINT ( 'NONE',  ( -79.39999999999999147, -34.25624999877096855, 101.7320508075688537 ) ) ;
#7934 = DIRECTION ( 'NONE',  ( -0.000000000000000000, -0.000000000000000000, -1.000000000000000000 ) ) ;
#7935 = CARTESIAN_POINT ( 'NONE',  ( 0.3126073911696399255, 2.020725942163686728, -3.499999999999999556 ) ) ;
#7936 = CARTESIAN_POINT ( 'NONE',  ( 85.15643035625001289, -32.99062499938548854, -98.40857419181659793 ) ) ;
#7937 = CARTESIAN_POINT ( 'NONE',  ( -82.40000000000001990, -34.16250000000000853, 97.00000000000000000 ) ) ;
#7938 = CARTESIAN_POINT ( 'NONE',  ( -82.39999999999999147, -33.40312499938548285, 96.81714838363319586 ) ) ;
#7939 =( BOUNDED_CURVE ( )  B_SPLINE_CURVE ( 2, ( #6235, #16775, #18151, #13831, #4773, #18247, #3389, #9341, #15304 ),
 .UNSPECIFIED., .F., .T. ) 
 B_SPLINE_CURVE_WITH_KNOTS ( ( 3, 2, 2, 2, 3 ),
 ( 0.4375000000000001110, 0.4444444444444444198, 0.4583333333333333148, 0.4722222222222222099, 0.4791666666666666852 ),
 .UNSPECIFIED. ) 
 CURVE ( )  GEOMETRIC_REPRESENTATION_ITEM ( )  RATIONAL_B_SPLINE_CURVE ( ( 0.9330127018922194093, 0.9330127018922204085, 1.000000000000000000, 0.8660254037844387076, 1.000000000000000000, 0.8660254037844387076, 1.000000000000000000, 0.9330127018922190762, 0.9330127018922194093 ) ) 
 REPRESENTATION_ITEM ( '' )  );
#7940 = CARTESIAN_POINT ( 'NONE',  ( 82.39999999999999147, -33.85312499938547859, -96.81714838363319586 ) ) ;
#7941 = ORIENTED_EDGE ( 'NONE', *, *, #2702, .F. ) ;
#7942 = CARTESIAN_POINT ( 'NONE',  ( 229.5999999999999375, -32.69999999999999574, -50.00000000000011369 ) ) ;
#7943 = DIRECTION ( 'NONE',  ( 1.000000000000000000, 0.000000000000000000, -0.000000000000000000 ) ) ;
#7944 = CARTESIAN_POINT ( 'NONE',  ( -82.39999999999999147, -30.78750000000000142, 102.9999999999999858 ) ) ;
#7945 = CARTESIAN_POINT ( 'NONE',  ( 235.3564303562499447, -33.21562499938548285, 101.5914258081833879 ) ) ;
#7946 = CARTESIAN_POINT ( 'NONE',  ( -82.39999999999999147, -31.71562499938548640, 96.81714838363319586 ) ) ;
#7947 = CARTESIAN_POINT ( 'NONE',  ( 235.3564303562499447, -33.21562499938548285, -48.40857419181671162 ) ) ;
#7948 = CARTESIAN_POINT ( 'NONE',  ( -85.40000000000000568, -32.73750000000000426, 98.26794919243111792 ) ) ;
#7949 = EDGE_LOOP ( 'NONE', ( #1957, #3162, #13902, #4376, #8444, #13666, #2943, #10642, #1306, #12008, #5989, #5968, #1440, #4791, #4819, #8021, #13357 ) ) ;
#7950 = APPLICATION_CONTEXT ( 'automotive_design' ) ;
#7951 = CARTESIAN_POINT ( 'NONE',  ( -81.62788447605926478, -34.99865355507268561, 102.9198516826838130 ) ) ;
#7952 = CARTESIAN_POINT ( 'NONE',  ( 244.7999999999999545, -29.80000000000002203, 147.7999999999999829 ) ) ;
#7953 = CARTESIAN_POINT ( 'NONE',  ( 79.64356964375001269, -32.20312499938548001, 98.40857419181659793 ) ) ;
#7954 = CARTESIAN_POINT ( 'NONE',  ( 84.53225329756206463, -31.99999999999999289, -98.24409948398914594 ) ) ;
#7955 = CARTESIAN_POINT ( 'NONE',  ( -85.15643035625001289, -32.01562499938548001, 101.5914258081833879 ) ) ;
#7956 = CARTESIAN_POINT ( 'NONE',  ( -85.15643035625001289, -32.05312499938548854, -99.99999999999998579 ) ) ;
#7957 = CARTESIAN_POINT ( 'NONE',  ( 79.64356964375001269, -34.04062499938549280, 101.5914258081833879 ) ) ;
#7958 = CARTESIAN_POINT ( 'NONE',  ( 85.15643035625001289, -32.50312499938548427, -99.99999999999998579 ) ) ;
#7959 = ADVANCED_FACE ( 'NONE', ( #2239 ), #5284, .T. ) ;
#7960 = CARTESIAN_POINT ( 'NONE',  ( 229.8435696437499871, -30.17812499938547433, -51.59142580818350865 ) ) ;
#7961 = CARTESIAN_POINT ( 'NONE',  ( -81.02178482187500208, -33.10312499938548569, 97.61286128772489690 ) ) ;
#7962 = CARTESIAN_POINT ( 'NONE',  ( -82.39999999999999147, -34.64062499938548711, -96.81714838363319586 ) ) ;
#7963 = ORIENTED_EDGE ( 'NONE', *, *, #15183, .T. ) ;
#7964 = CARTESIAN_POINT ( 'NONE',  ( 85.15643035624999868, -33.44062499938548427, 101.5914258081833879 ) ) ;
#7965 = CARTESIAN_POINT ( 'NONE',  ( -82.39999999999999147, -32.98124999877096286, 102.9999999999999858 ) ) ;
#7966 = AXIS2_PLACEMENT_3D ( 'NONE', #16680, #6615, #10907 ) ;
#7967 = CARTESIAN_POINT ( 'NONE',  ( -82.39999999999999147, -31.15312499938548640, 96.81714838363319586 ) ) ;
#7968 = CARTESIAN_POINT ( 'NONE',  ( -85.15643035624999868, -34.26562499938548711, 101.5914258081833879 ) ) ;
#7969 = ORIENTED_EDGE ( 'NONE', *, *, #5907, .F. ) ;
#7970 = CARTESIAN_POINT ( 'NONE',  ( -82.39999999999999147, -33.03750000000000142, -96.53589838486223584 ) ) ;
#7971 =( BOUNDED_CURVE ( )  B_SPLINE_CURVE ( 2, ( #9447, #481, #10916, #12291, #5262, #18446, #4874, #2022, #6624 ),
 .UNSPECIFIED., .F., .F. ) 
 B_SPLINE_CURVE_WITH_KNOTS ( ( 3, 2, 2, 2, 3 ),
 ( 0.7291666666666666297, 0.7361111111111111605, 0.7500000000000000000, 0.7638888888888888395, 0.7708333333333331483 ),
 .UNSPECIFIED. ) 
 CURVE ( )  GEOMETRIC_REPRESENTATION_ITEM ( )  RATIONAL_B_SPLINE_CURVE ( ( 0.9330127018922192983, 0.9330127018922187432, 1.000000000000000000, 0.8660254037844387076, 1.000000000000000000, 0.8660254037844387076, 1.000000000000000000, 0.9330127018922209636, 0.9330127018922194093 ) ) 
 REPRESENTATION_ITEM ( '' )  );
#7972 = CARTESIAN_POINT ( 'NONE',  ( 231.0999999999999375, -34.36874999877096570, -47.40192378864679768 ) ) ;
#7973 = PLANE ( 'NONE',  #7344 ) ;
#7974 = CARTESIAN_POINT ( 'NONE',  ( 232.5999999999999659, -32.53124999877096712, -47.00000000000011369 ) ) ;
#7975 = CARTESIAN_POINT ( 'NONE',  ( 231.2217848218749339, -34.82812499938548001, 97.61286128772489690 ) ) ;
#7976 = CARTESIAN_POINT ( 'NONE',  ( -83.90000000000000568, -34.52268749875867826, 97.40192378864668399 ) ) ;
#7977 = EDGE_CURVE ( 'NONE', #17634, #12136, #14744, .T. ) ;
#7978 = ORIENTED_EDGE ( 'NONE', *, *, #19168, .F. ) ;
#7979 = CYLINDRICAL_SURFACE ( 'NONE', #9929, 3.000000000000002665 ) ;
#7980 = CARTESIAN_POINT ( 'NONE',  ( 244.7999999999999545, -35.00000000000000000, -100.0000000000000000 ) ) ;
#7981 = CARTESIAN_POINT ( 'NONE',  ( -85.40000000000000568, -33.54374999877096286, -99.99999999999998579 ) ) ;
#7982 = DIRECTION ( 'NONE',  ( -0.000000000000000000, -0.000000000000000000, -1.000000000000000000 ) ) ;
#7983 = VECTOR ( 'NONE', #18061, 1000.000000000000000 ) ;
#7984 = FACE_OUTER_BOUND ( 'NONE', #9771, .T. ) ;
#7985 = CARTESIAN_POINT ( 'NONE',  ( 84.69813954184694182, -35.39427337414329600, -98.07164457472185859 ) ) ;
#7986 = DIRECTION ( 'NONE',  ( -1.000000000000000000, -0.000000000000000000, -0.000000000000000000 ) ) ;
#7987 = ORIENTED_EDGE ( 'NONE', *, *, #3851, .T. ) ;
#7988 = CARTESIAN_POINT ( 'NONE',  ( 233.9782151781249411, -34.60312499938548569, -47.61286128772501769 ) ) ;
#7989 = CONTEXT_DEPENDENT_SHAPE_REPRESENTATION ( #3208, #11064 ) ;
#7990 = CARTESIAN_POINT ( 'NONE',  ( 235.3564303562499447, -33.14062499938548001, 98.40857419181659793 ) ) ;
#7991 = CARTESIAN_POINT ( 'NONE',  ( 229.8435696437499871, -31.19062499938548072, -51.59142580818350865 ) ) ;
#7992 = PRESENTATION_LAYER_ASSIGNMENT (  '', '', ( #17992 ) ) ;
#7993 = CARTESIAN_POINT ( 'NONE',  ( -81.02178482187500208, -32.69062499938548427, 102.3871387122750889 ) ) ;
#7994 = VERTEX_POINT ( 'NONE', #15434 ) ;
#7995 = ORIENTED_EDGE ( 'NONE', *, *, #18683, .T. ) ;
#7996 = CARTESIAN_POINT ( 'NONE',  ( -85.15643035625001289, -31.49062499938548498, -99.99999999999998579 ) ) ;
#7997 = CARTESIAN_POINT ( 'NONE',  ( -82.40000000000000568, -30.95624999877097139, 96.99999999999998579 ) ) ;
#7998 = DIRECTION ( 'NONE',  ( 0.000000000000000000, -1.000000000000000000, 0.000000000000000000 ) ) ;
#7999 = EDGE_LOOP ( 'NONE', ( #517, #3474, #11002, #14020 ) ) ;
#8000 = CARTESIAN_POINT ( 'NONE',  ( 83.77821517812500929, -32.12812499938548427, 102.3871387122750889 ) ) ;
#8001 = EDGE_CURVE ( 'NONE', #1272, #10334, #16140, .T. ) ;
#8002 = CARTESIAN_POINT ( 'NONE',  ( -80.90000000000000568, -34.29374999877096997, -97.40192378864668399 ) ) ;
#8003 = CARTESIAN_POINT ( 'NONE',  ( -82.17437583783126342, -34.99999999999998579, 97.01974242045221786 ) ) ;
#8004 = CARTESIAN_POINT ( 'NONE',  ( -80.90000000000000568, -33.24374999877097281, 97.40192378864668399 ) ) ;
#8005 = CARTESIAN_POINT ( 'NONE',  ( -80.90000000000000568, -35.04374999877096997, 97.40192378864668399 ) ) ;
#8006 = CARTESIAN_POINT ( 'NONE',  ( 84.06832524826556607, -34.99999999999999289, -102.2567273996575210 ) ) ;
#8007 = CARTESIAN_POINT ( 'NONE',  ( 229.5999999999999375, -33.95624999877096428, -48.26794919243123161 ) ) ;
#8008 = FACE_OUTER_BOUND ( 'NONE', #7226, .T. ) ;
#8009 = CARTESIAN_POINT ( 'NONE',  ( 231.7447645400923193, -35.19352049914630953, 96.73097394877602540 ) ) ;
#8010 = ORIENTED_EDGE ( 'NONE', *, *, #9607, .F. ) ;
#8011 = DIRECTION ( 'NONE',  ( 1.000000000000000000, 3.548298019043479384E-15, 0.000000000000000000 ) ) ;
#8012 = CARTESIAN_POINT ( 'NONE',  ( 231.0999999999999375, -32.26874999877096428, 97.40192378864668399 ) ) ;
#8013 = ORIENTED_EDGE ( 'NONE', *, *, #16891, .F. ) ;
#8014 = CARTESIAN_POINT ( 'NONE',  ( -83.90000000000000568, -33.61874999877097281, 97.40192378864668399 ) ) ;
#8015 = DIRECTION ( 'NONE',  ( 0.000000000000000000, 0.000000000000000000, -1.000000000000000000 ) ) ;
#8016 = UNCERTAINTY_MEASURE_WITH_UNIT (LENGTH_MEASURE( 1.000000000000000082E-05 ), #2342, 'distance_accuracy_value', 'NONE');
#8017 = CARTESIAN_POINT ( 'NONE',  ( 2.687328764639642653, -3.067272167851299969, -0.05923475698271395140 ) ) ;
#8018 = ORIENTED_EDGE ( 'NONE', *, *, #11887, .T. ) ;
#8019 = CARTESIAN_POINT ( 'NONE',  ( 233.9782151781249411, -34.79062499938547859, -52.38713871227520968 ) ) ;
#8020 = ORIENTED_EDGE ( 'NONE', *, *, #13997, .F. ) ;
#8021 = ORIENTED_EDGE ( 'NONE', *, *, #11281, .F. ) ;
#8022 =( BOUNDED_CURVE ( )  B_SPLINE_CURVE ( 2, ( #15275, #8240, #8141, #16938, #18408, #9706, #535, #18604, #16846, #14190, #5218, #4931, #6491, #12533, #11066, #1988, #14093, #11168, #6786, #3550, #12440, #6586, #18703, #637, #6392, #3450, #2085, #18312, #15572, #15372, #12734, #5028, #5322, #7945, #15473, #2185, #17229, #13897, #1890, #7848, #9506, #8041, #13999, #7059, #5789, #15863, #2470, #11650, #13204, #4131, #17610, #1018, #13018, #923, #12922, #14566, #14379, #18795, #5611, #13109, #5420, #1203, #19176, #17518, #14470, #12828, #5698, #4226, #19079, #18990, #6880, #7160, #11360, #15763, #9801, #17325, #10182, #14667, #3833, #16145, #3934, #8615, #2758 ),
 .UNSPECIFIED., .F., .F. ) 
 B_SPLINE_CURVE_WITH_KNOTS ( ( 3, 2, 2, 2, 2, 2, 2, 2, 2, 2, 2, 2, 2, 2, 2, 2, 2, 2, 2, 2, 2, 2, 2, 2, 2, 2, 2, 2, 2, 2, 2, 2, 2, 2, 2, 2, 2, 2, 2, 2, 2, 3 ),
 ( 0.3495698921800969305, 0.3600184345287980592, 0.3750192026341646057, 0.3900199707395312076, 0.4050207388448978096, 0.4200215069502644116, 0.4350222750556310136, 0.4500230431609976156, 0.4650238112663641621, 0.4800245793717307086, 0.4950253474770973661, 0.5100261155824639125, 0.5250268836878304590, 0.5400276517931971165, 0.5550284198985636630, 0.5700291880039303205, 0.5850299561092967560, 0.6000307242146634135, 0.6150314923200299599, 0.6300322604253966174, 0.6450330285307631639, 0.6600337966361298214, 0.6750345647414963679, 0.6900353328468629144, 0.7050361009522295719, 0.7200368690575961184, 0.7350376371629627759, 0.7500384052683293223, 0.7650391733736958688, 0.7800399414790624153, 0.7950407095844291838, 0.8100414776897956193, 0.8250422457951621658, 0.8400430139005288233, 0.8550437820058953697, 0.8700445501112620272, 0.8850453182166285737, 0.9000460863219952312, 0.9150468544273617777, 0.9300476225327284352, 0.9450483906380949817, 0.9496006163947608991 ),
 .UNSPECIFIED. ) 
 CURVE ( )  GEOMETRIC_REPRESENTATION_ITEM ( )  RATIONAL_B_SPLINE_CURVE ( ( 0.9433623850486696494, 0.9066821623815634057, 1.000000000000000000, 0.8660254037844387076, 1.000000000000000000, 0.8660254037844387076, 1.000000000000000000, 0.8660254037844387076, 1.000000000000000000, 0.8660254037844387076, 1.000000000000000000, 0.8660254037844387076, 1.000000000000000000, 0.8660254037844387076, 1.000000000000000000, 0.8660254037844387076, 1.000000000000000000, 0.8660254037844387076, 1.000000000000000000, 0.8660254037844387076, 1.000000000000000000, 0.8660254037844387076, 1.000000000000000000, 0.8660254037844387076, 1.000000000000000000, 0.8660254037844387076, 1.000000000000000000, 0.8660254037844387076, 1.000000000000000000, 0.8660254037844387076, 1.000000000000000000, 0.8660254037844387076, 1.000000000000000000, 0.8660254037844387076, 1.000000000000000000, 0.8660254037844387076, 1.000000000000000000, 0.8660254037844387076, 1.000000000000000000, 0.8660254037844387076, 1.000000000000000000, 0.8660254037844387076, 1.000000000000000000, 0.8660254037844387076, 1.000000000000000000, 0.8660254037844387076, 1.000000000000000000, 0.8660254037844387076, 1.000000000000000000, 0.8660254037844387076, 1.000000000000000000, 0.8660254037844387076, 1.000000000000000000, 0.8660254037844387076, 1.000000000000000000, 0.8660254037844387076, 1.000000000000000000, 0.8660254037844387076, 1.000000000000000000, 0.8660254037844387076, 1.000000000000000000, 0.8660254037844387076, 1.000000000000000000, 0.8660254037844387076, 1.000000000000000000, 0.8660254037844387076, 1.000000000000000000, 0.8660254037844387076, 1.000000000000000000, 0.8660254037844387076, 1.000000000000000000, 0.8660254037844387076, 1.000000000000000000, 0.8660254037844387076, 1.000000000000000000, 0.8660254037844387076, 1.000000000000000000, 0.8660254037844387076, 1.000000000000000000, 0.8660254037844387076, 1.000000000000000000, 0.9593432414028713051, 0.9433623850486665408 ) ) 
 REPRESENTATION_ITEM ( '' )  );
#8023 = CARTESIAN_POINT ( 'NONE',  ( 232.5999999999999375, -33.26249999999999574, -53.00000000000011369 ) ) ;
#8024 = CARTESIAN_POINT ( 'NONE',  ( 85.40000000000000568, -30.03750000000000497, -98.26794919243111792 ) ) ;
#8025 = FACE_OUTER_BOUND ( 'NONE', #16887, .T. ) ;
#8026 = VECTOR ( 'NONE', #12669, 1000.000000000000000 ) ;
#8027 = CARTESIAN_POINT ( 'NONE',  ( -79.39999999999999147, -35.08124999877097139, 98.26794919243110371 ) ) ;
#8028 = CARTESIAN_POINT ( 'NONE',  ( -79.39999999999999147, -34.27106250001229171, 99.99999999999998579 ) ) ;
#8029 = CARTESIAN_POINT ( 'NONE',  ( -83.20384757729335945, -32.28615380933863577, -103.0000000000000000 ) ) ;
#8030 = CARTESIAN_POINT ( 'NONE',  ( 244.7999999999999545, -29.80000000000000782, -100.0000000000000000 ) ) ;
#8031 = CARTESIAN_POINT ( 'NONE',  ( 83.77821517812500929, -33.47812499938548569, -97.61286128772489690 ) ) ;
#8032 = CIRCLE ( 'NONE', #2106, 4.000000000000000000 ) ;
#8033 = CARTESIAN_POINT ( 'NONE',  ( -81.02178482187500208, -34.04062499938548569, 102.3871387122750889 ) ) ;
#8034 = ADVANCED_FACE ( 'NONE', ( #8298 ), #14437, .F. ) ;
#8035 = CARTESIAN_POINT ( 'NONE',  ( 79.64356964375001269, -33.47812499938547859, -98.40857419181659793 ) ) ;
#8036 = ORIENTED_EDGE ( 'NONE', *, *, #10539, .F. ) ;
#8037 = CARTESIAN_POINT ( 'NONE',  ( 229.5999999999999375, -32.24999999999999289, -50.00000000000011369 ) ) ;
#8038 = CARTESIAN_POINT ( 'NONE',  ( -79.39999999999999147, -34.23750000000000426, 98.26794919243110371 ) ) ;
#8039 = VECTOR ( 'NONE', #9994, 1000.000000000000000 ) ;
#8040 = CARTESIAN_POINT ( 'NONE',  ( -85.40000000000000568, -33.99374999877097281, 99.99999999999998579 ) ) ;
#8041 = CARTESIAN_POINT ( 'NONE',  ( 232.5999999999999943, -33.51562499938548001, 96.81714838363319586 ) ) ;
#8042 = CARTESIAN_POINT ( 'NONE',  ( -82.39999999999999147, -31.26562499938549067, 96.81714838363319586 ) ) ;
#8043 = CARTESIAN_POINT ( 'NONE',  ( 229.8435696437499871, -33.44062499938547717, -51.59142580818350865 ) ) ;
#8044 = CARTESIAN_POINT ( 'NONE',  ( -82.39999999999999147, -32.13749999999999574, 103.4641016151377499 ) ) ;
#8045 = EDGE_CURVE ( 'NONE', #15137, #4556, #2618, .T. ) ;
#8046 = ORIENTED_EDGE ( 'NONE', *, *, #11635, .T. ) ;
#8047 = CARTESIAN_POINT ( 'NONE',  ( 4.158806752148102248, -2.089318365061878069, 3.500000000000000000 ) ) ;
#8048 = AXIS2_PLACEMENT_3D ( 'NONE', #9236, #13633, #467 ) ;
#8049 = CARTESIAN_POINT ( 'NONE',  ( 80.07894310789828296, -34.99999999999997868, 98.50261820439547478 ) ) ;
#8050 = CARTESIAN_POINT ( 'NONE',  ( 85.15643035624999868, -33.32812499938548001, 101.5914258081833879 ) ) ;
#8051 = VECTOR ( 'NONE', #15050, 1000.000000000000000 ) ;
#8052 = AXIS2_PLACEMENT_3D ( 'NONE', #15359, #7934, #5018 ) ;
#8053 = DIRECTION ( 'NONE',  ( 1.000000000000000000, 0.000000000000000000, 0.000000000000000000 ) ) ;
#8054 =( BOUNDED_CURVE ( )  B_SPLINE_CURVE ( 2, ( #5590, #16228, #8594, #14945, #1466, #8881, #16319, #1570, #1280 ),
 .UNSPECIFIED., .F., .F. ) 
 B_SPLINE_CURVE_WITH_KNOTS ( ( 3, 2, 2, 2, 3 ),
 ( 0.7708333333333332593, 0.7777777777777777901, 0.7916666666666666297, 0.8055555555555555802, 0.8125000000000000000 ),
 .UNSPECIFIED. ) 
 CURVE ( )  GEOMETRIC_REPRESENTATION_ITEM ( )  RATIONAL_B_SPLINE_CURVE ( ( 0.9330127018922192983, 0.9330127018922187432, 1.000000000000000000, 0.8660254037844387076, 1.000000000000000000, 0.8660254037844387076, 1.000000000000000000, 0.9330127018922194093, 0.9330127018922194093 ) ) 
 REPRESENTATION_ITEM ( '' )  );
#8055 = EDGE_CURVE ( 'NONE', #15743, #15327, #15510, .T. ) ;
#8056 = CARTESIAN_POINT ( 'NONE',  ( -79.64356964374999848, -31.37812499938548427, 99.99999999999998579 ) ) ;
#8057 = CARTESIAN_POINT ( 'NONE',  ( 81.45486068924893175, -32.00000000000000000, 97.24663084804296886 ) ) ;
#8058 = CARTESIAN_POINT ( 'NONE',  ( 85.15643035624999868, -33.32812499938548001, 101.5914258081833879 ) ) ;
#8059 = ADVANCED_FACE ( 'NONE', ( #10432 ), #18065, .F. ) ;
#8060 = CARTESIAN_POINT ( 'NONE',  ( 81.02178482187500208, -31.90312499938548996, -102.3871387122750889 ) ) ;
#8061 = CARTESIAN_POINT ( 'NONE',  ( 229.8435696437499303, -30.14062499938548001, -50.00000000000011369 ) ) ;
#8062 = CARTESIAN_POINT ( 'NONE',  ( -79.64356964374998427, -34.11562499938548854, 101.5914258081833879 ) ) ;
#8063 = CARTESIAN_POINT ( 'NONE',  ( -79.64356964375001269, -34.04062499938549280, -101.5914258081833879 ) ) ;
#8064 = EDGE_CURVE ( 'NONE', #12906, #13062, #917, .T. ) ;
#8065 = ORIENTED_EDGE ( 'NONE', *, *, #5185, .T. ) ;
#8066 = CARTESIAN_POINT ( 'NONE',  ( 79.64356964375001269, -33.14062499938548711, 101.5914258081833879 ) ) ;
#8067 = CARTESIAN_POINT ( 'NONE',  ( 3.958484000407173298, -3.734437307742043632, -0.5317648453100631833 ) ) ;
#8068 = CIRCLE ( 'NONE', #18998, 3.000000000000002665 ) ;
#8069 = CARTESIAN_POINT ( 'NONE',  ( -79.64356964374999848, -31.71562499938548285, 99.99999999999998579 ) ) ;
#8070 = CARTESIAN_POINT ( 'NONE',  ( -83.77821517812500929, -33.77812499938548285, 102.3871387122750889 ) ) ;
#8071 = CYLINDRICAL_SURFACE ( 'NONE', #14292, 3.000000000000002665 ) ;
#8072 = ORIENTED_EDGE ( 'NONE', *, *, #15488, .T. ) ;
#8073 = CARTESIAN_POINT ( 'NONE',  ( -82.39999999999999147, -33.93750000000000000, -96.53589838486223584 ) ) ;
#8074 = CARTESIAN_POINT ( 'NONE',  ( 81.59615242270662350, -32.83259618943233704, -96.99999999999998579 ) ) ;
#8075 = CARTESIAN_POINT ( 'NONE',  ( 82.85024983566745505, -34.99999999999999289, -97.02690897175904183 ) ) ;
#8076 = EDGE_CURVE ( 'NONE', #12940, #17759, #2896, .T. ) ;
#8077 = DIRECTION ( 'NONE',  ( 0.000000000000000000, 0.000000000000000000, 1.000000000000000000 ) ) ;
#8078 = B_SPLINE_CURVE_WITH_KNOTS ( 'NONE', 3,
 ( #2020, #12768, #12476, #2126, #3774, #16972, #11300, #9347, #15310, #1923, #7886, #13837, #17460, #5457, #1338, #11683 ),
 .UNSPECIFIED., .F., .F.,
 ( 4, 2, 2, 2, 2, 2, 2, 4 ),
 ( 0.000000000000000000, 0.0005391024520905149430, 0.001078204904181029886, 0.002156409808361992118, 0.002695512260452471390, 0.003234614712542950229, 0.003773717164633429936, 0.004312819616723909642 ),
 .UNSPECIFIED. ) ;
#8079 = CARTESIAN_POINT ( 'NONE',  ( 231.2217848218749339, -30.21562499938547575, 97.61286128772489690 ) ) ;
#8080 = CARTESIAN_POINT ( 'NONE',  ( -85.40000000000000568, -33.99768749875867968, 99.99999999999998579 ) ) ;
#8081 = ORIENTED_EDGE ( 'NONE', *, *, #4601, .T. ) ;
#8082 = FACE_OUTER_BOUND ( 'NONE', #15843, .T. ) ;
#8083 = CARTESIAN_POINT ( 'NONE',  ( 82.40000000000001990, -32.13750000000000284, 97.00000000000000000 ) ) ;
#8084 = CARTESIAN_POINT ( 'NONE',  ( 81.02178482187500208, -34.79062499938548569, 102.3871387122750889 ) ) ;
#8085 = DIRECTION ( 'NONE',  ( 7.222237291452147586E-32, -1.214306433183764966E-16, 1.000000000000000000 ) ) ;
#8086 = CYLINDRICAL_SURFACE ( 'NONE', #9572, 3.000000000000002665 ) ;
#8087 = B_SPLINE_CURVE_WITH_KNOTS ( 'NONE', 3,
 ( #14795, #16180, #2790, #11771 ),
 .UNSPECIFIED., .F., .F.,
 ( 4, 4 ),
 ( 0.002080789711329297104, 0.004173039763574517766 ),
 .UNSPECIFIED. ) ;
#8088 = CARTESIAN_POINT ( 'NONE',  ( 82.39999999999999147, -30.59062499938548640, -103.1828516163667899 ) ) ;
#8089 = CARTESIAN_POINT ( 'NONE',  ( 232.5999999999999375, -34.83749999999999147, 103.4641016151377499 ) ) ;
#8090 = ORIENTED_EDGE ( 'NONE', *, *, #1401, .F. ) ;
#8091 = CARTESIAN_POINT ( 'NONE',  ( 80.90000000000000568, -31.59374999877097423, 97.40192378864668399 ) ) ;
#8092 = CARTESIAN_POINT ( 'NONE',  ( 235.3564303562499447, -32.69062499938547717, 98.40857419181659793 ) ) ;
#8093 = EDGE_CURVE ( 'NONE', #800, #2879, #7518, .T. ) ;
#8094 = CARTESIAN_POINT ( 'NONE',  ( 235.5999999999999943, -34.70624999877096428, -48.26794919243124582 ) ) ;
#8095 =( BOUNDED_CURVE ( )  B_SPLINE_CURVE ( 2, ( #18736, #5356, #18635, #18925, #11494, #4069, #1138, #5258, #11204 ),
 .UNSPECIFIED., .F., .F. ) 
 B_SPLINE_CURVE_WITH_KNOTS ( ( 3, 2, 2, 2, 3 ),
 ( 0.8125000000000001110, 0.8194444444444444198, 0.8333333333333333703, 0.8472222222222222099, 0.8530683953269213582 ),
 .UNSPECIFIED. ) 
 CURVE ( )  GEOMETRIC_REPRESENTATION_ITEM ( )  RATIONAL_B_SPLINE_CURVE ( ( 0.9330127018922194093, 0.9330127018922204085, 1.000000000000000000, 0.8660254037844387076, 1.000000000000000000, 0.8660254037844387076, 1.000000000000000000, 0.9436068149601996025, 0.9346881722405915305 ) ) 
 REPRESENTATION_ITEM ( '' )  );
#8096 = CARTESIAN_POINT ( 'NONE',  ( -81.02178482187500208, -34.49062499938548854, 102.3871387122750889 ) ) ;
#8097 = CARTESIAN_POINT ( 'NONE',  ( 235.5999999999999943, -34.76249999999999574, -48.26794919243124582 ) ) ;
#8098 = ORIENTED_EDGE ( 'NONE', *, *, #1251, .F. ) ;
#8099 = ORIENTED_EDGE ( 'NONE', *, *, #16055, .T. ) ;
#8100 = CARTESIAN_POINT ( 'NONE',  ( -83.77821517812500929, -30.96562499938548640, -97.61286128772489690 ) ) ;
#8101 = CYLINDRICAL_SURFACE ( 'NONE', #4431, 5.199999999999996625 ) ;
#8102 = ORIENTED_EDGE ( 'NONE', *, *, #1534, .T. ) ;
#8103 = CARTESIAN_POINT ( 'NONE',  ( 79.64356964374998427, -33.14062499938548711, 101.5914258081833879 ) ) ;
#8104 = CARTESIAN_POINT ( 'NONE',  ( -79.39999999999999147, -32.86874999877097281, -99.99999999999998579 ) ) ;
#8105 = CARTESIAN_POINT ( 'NONE',  ( 79.39999999999999147, -32.96250000000000568, 98.26794919243113213 ) ) ;
#8106 = CARTESIAN_POINT ( 'NONE',  ( -85.15643035625001289, -35.20312499938548711, 99.99999999999998579 ) ) ;
#8107 = CARTESIAN_POINT ( 'NONE',  ( -80.90000000000000568, -31.89374999877096784, 97.40192378864668399 ) ) ;
#8108 = CARTESIAN_POINT ( 'NONE',  ( -85.40000000000000568, -33.95624999877097139, 101.7320508075688679 ) ) ;
#8109 = CARTESIAN_POINT ( 'NONE',  ( 85.31192385480649421, -34.99999999999999289, -99.60674545263997004 ) ) ;
#8110 = CARTESIAN_POINT ( 'NONE',  ( 82.40000000000000568, -30.00000000000000355, -99.99999999999998579 ) ) ;
#8111 = DIRECTION ( 'NONE',  ( 7.222237291452147586E-32, -1.214306433183764966E-16, 1.000000000000000000 ) ) ;
#8112 = CARTESIAN_POINT ( 'NONE',  ( 231.2217848218749339, -34.56562499938547717, 102.3871387122750889 ) ) ;
#8113 = ORIENTED_EDGE ( 'NONE', *, *, #13406, .F. ) ;
#8114 = CARTESIAN_POINT ( 'NONE',  ( 83.77821517812500929, -32.01562499938548001, -97.61286128772489690 ) ) ;
#8115 = CARTESIAN_POINT ( 'NONE',  ( -82.39999999999999147, -34.75312499938549138, -103.1828516163667899 ) ) ;
#8116 = FACE_BOUND ( 'NONE', #795, .T. ) ;
#8117 = ORIENTED_EDGE ( 'NONE', *, *, #2244, .T. ) ;
#8118 = LINE ( 'NONE', #708, #1784 ) ;
#8119 = FACE_OUTER_BOUND ( 'NONE', #16655, .T. ) ;
#8120 = CARTESIAN_POINT ( 'NONE',  ( 82.40000000000001990, -32.13750000000000284, 97.00000000000000000 ) ) ;
#8121 = ORIENTED_EDGE ( 'NONE', *, *, #4980, .T. ) ;
#8122 = CARTESIAN_POINT ( 'NONE',  ( 1.734723475976807094E-15, 4.618802153517012954, -0.4999999999999995559 ) ) ;
#8123 = CARTESIAN_POINT ( 'NONE',  ( 4.101954839143203912, -2.368264730583031330, -3.681130640444377988 ) ) ;
#8124 = ORIENTED_EDGE ( 'NONE', *, *, #15182, .F. ) ;
#8125 = B_SPLINE_CURVE_WITH_KNOTS ( 'NONE', 3,
 ( #5630, #1037, #1225, #17447, #4058 ),
 .UNSPECIFIED., .F., .F.,
 ( 4, 1, 4 ),
 ( 0.000000000000000000, 0.002020725942163688338, 0.004041451884327376676 ),
 .UNSPECIFIED. ) ;
#8126 = CARTESIAN_POINT ( 'NONE',  ( -79.39999999999999147, -32.02500000000000568, -99.99999999999998579 ) ) ;
#8127 = CARTESIAN_POINT ( 'NONE',  ( 83.25523545990762386, -35.19352049914630953, -96.73097394877602540 ) ) ;
#8128 = CARTESIAN_POINT ( 'NONE',  ( -4.000000000000000000, -1.560351142792950618, -0.2242961665059814425 ) ) ;
#8129 = CARTESIAN_POINT ( 'NONE',  ( -79.39999999999999147, -33.76874999877097139, 99.99999999999998579 ) ) ;
#8130 = CARTESIAN_POINT ( 'NONE',  ( -80.90000000000000568, -30.15000000000000213, 97.40192378864668399 ) ) ;
#8131 = LINE ( 'NONE', #14083, #13354 ) ;
#8132 = CARTESIAN_POINT ( 'NONE',  ( 79.39999999999999147, -33.35624999877096997, 98.26794919243113213 ) ) ;
#8133 = CARTESIAN_POINT ( 'NONE',  ( 79.64356964374999848, -32.27812499938548996, -99.99999999999998579 ) ) ;
#8134 = CARTESIAN_POINT ( 'NONE',  ( -99.99999999999998579, -32.00000000000000000, -150.0000000000000000 ) ) ;
#8135 = CARTESIAN_POINT ( 'NONE',  ( -81.02178482187500208, -34.34062499938548285, 97.61286128772489690 ) ) ;
#8136 = CARTESIAN_POINT ( 'NONE',  ( 83.77821517812500929, -35.01562499938548711, -102.3871387122750889 ) ) ;
#8137 = ORIENTED_EDGE ( 'NONE', *, *, #12958, .T. ) ;
#8138 = CARTESIAN_POINT ( 'NONE',  ( 230.9855258467272563, -35.02670941564509377, -52.74312242118950422 ) ) ;
#8139 = CARTESIAN_POINT ( 'NONE',  ( -82.39999999999999147, -34.16250000000000142, 96.53589838486223584 ) ) ;
#8140 = DIRECTION ( 'NONE',  ( 0.000000000000000000, 0.000000000000000000, 1.000000000000000000 ) ) ;
#8141 = CARTESIAN_POINT ( 'NONE',  ( 229.8435696437499303, -32.05312499938548143, 99.99999999999998579 ) ) ;
#8142 = CARTESIAN_POINT ( 'NONE',  ( -83.77821517812500929, -34.67812499938548854, 102.3871387122750889 ) ) ;
#8143 = CARTESIAN_POINT ( 'NONE',  ( 232.5999999999999375, -34.86562499938548143, -53.18285161636690361 ) ) ;
#8144 = CARTESIAN_POINT ( 'NONE',  ( -82.39999999999999147, -32.36250000000000426, 96.53589838486223584 ) ) ;
#8145 = VERTEX_POINT ( 'NONE', #3395 ) ;
#8146 = CARTESIAN_POINT ( 'NONE',  ( -83.20395887649183919, -35.00000000000001421, -97.36341917746362640 ) ) ;
#8147 =( BOUNDED_SURFACE ( )  B_SPLINE_SURFACE ( 1, 2, ( 
 ( #5259, #5357, #2593, #14505, #11587, #1050, #3873, #17552, #2404, #5548, #8368, #17360, #959, #3969, #12863, #9936, #2499, #7002, #2795, #1530, #17839, #16372, #2888, #5733, #10318, #19315, #6020, #5926, #5828, #4454, #11969, #10408, #8936, #14607, #11682, #3077, #17649, #11872, #4262, #11779, #14800, #7480, #14902, #9037, #17753, #7380, #15002, #14700, #1337, #67, #1238, #17937, #7190, #10221, #1427, #16187, #4358, #13436, #16278, #13340, #8844, #4549, #2980, #10505, #16472, #19113, #13139, #8748, #7284, #13238, #19211, #15768, #17524, #17330, #14571, #11365, #16153, #18708, #11561, #12926, #17432, #10098, #12835, #2765, #4136, #1208, #6885, #2659, #5425, #8431, #8620, #5329, #14476, #3939, #15957, #9906, #16054, #7165, #8526, #1106, #2562, #7064, #15869, #6975, #2475, #13115, #13023, #4043, #14384, #19086, #1023, #18897, #5705, #5517, #11465, #11656, #17234, #2376, #10002, #17618, #18995, #929, #12740, #4233, #5616, #10191, #18801, #8721, #14674, #1309, #11267, #3839, #9806, #8337, #14294, #17814, #18011 ),
 ( #4625, #10578, #233, #14973, #9197, #1687, #13212, #141, #15160, #4519, #16635, #17913, #4332, #7451, #3142, #18109, #7354, #9103, #13502, #12038, #5991, #10292, #13410, #1597, #13593, #9013, #2955, #6091, #16543, #4424, #10477, #10383, #15066, #7544, #16442, #8909, #19183, #40, #5900, #6190, #4721, #11846, #16252, #7639, #16345, #12140, #14871, #10665, #5798, #3239, #11942, #3051, #7257, #13310, #11750, #17721, #2861, #1402, #8818, #19284, #1499, #14774, #6809, #9822, #2393, #15978, #5242, #15885, #12943, #14494, #2679, #2490, #15784, #17448, #7084, #2582, #11577, #1226, #18724, #8355, #14309, #11191, #15691, #13040, #17348, #9727, #1038, #3860, #19011, #17154, #10019, #14400, #946, #8637, #8543, #11382, #4156, #3762, #5631, #10116, #5345, #16071, #2294, #8448, #14594, #17540, #18914, #6992, #12755, #11285, #12651, #18624, #1126, #8259, #14209, #5533, #846, #17253, #6901, #11482, #12850, #9924, #18821, #3958, #5444, #4059, #3067, #18031, #7273, #9029, #13427, #11957, #5916, #4251, #13327, #14889, #13518 ) ),
 .UNSPECIFIED., .F., .F., .F. ) 
 B_SPLINE_SURFACE_WITH_KNOTS ( ( 2, 2 ),
 ( 3, 2, 2, 2, 2, 2, 2, 2, 2, 2, 2, 2, 2, 2, 2, 2, 2, 2, 2, 2, 2, 2, 2, 2, 2, 2, 2, 2, 2, 2, 2, 2, 2, 2, 2, 2, 2, 2, 2, 2, 2, 2, 2, 2, 2, 2, 2, 2, 2, 2, 2, 2, 2, 2, 2, 2, 2, 2, 2, 2, 2, 2, 2, 2, 2, 2, 2, 2, 3 ),
 ( 0.000000000000000000, 1.000000000000000000 ),
 ( 0.000000000000000000, 0.01388888888888888812, 0.02777777777777777624, 0.04166666666666666435, 0.05555555555555555247, 0.06944444444444444753, 0.08333333333333332871, 0.09722222222222222376, 0.1111111111111111049, 0.1250000000000000000, 0.1388888888888888951, 0.1527777777777777901, 0.1666666666666666574, 0.1805555555555555525, 0.1944444444444444475, 0.2083333333333333426, 0.2222222222222222099, 0.2361111111111111049, 0.2500000000000000000, 0.2638888888888888951, 0.2777777777777777901, 0.2916666666666666852, 0.3055555555555555802, 0.3194444444444444198, 0.3333333333333333148, 0.3472222222222222099, 0.3611111111111111049, 0.3750000000000000000, 0.3888888888888888951, 0.4027777777777777901, 0.4166666666666666852, 0.4305555555555555802, 0.4444444444444444198, 0.4583333333333333148, 0.4722222222222222099, 0.4861111111111111049, 0.5000000000000000000, 0.5138888888888888395, 0.5277777777777777901, 0.5416666666666666297, 0.5555555555555555802, 0.5694444444444444198, 0.5833333333333333703, 0.5972222222222222099, 0.6111111111111111605, 0.6250000000000000000, 0.6388888888888888395, 0.6527777777777777901, 0.6666666666666666297, 0.6805555555555555802, 0.6944444444444444198, 0.7083333333333333703, 0.7222222222222222099, 0.7361111111111111605, 0.7500000000000000000, 0.7638888888888888395, 0.7777777777777777901, 0.7916666666666666297, 0.8055555555555555802, 0.8194444444444444198, 0.8333333333333333703, 0.8472222222222222099, 0.8611111111111111605, 0.8750000000000000000, 0.8888888888888888395, 0.9027777777777777901, 0.9166666666666666297, 0.9258785066912882389, 0.9351372917582011501 ),
 .UNSPECIFIED. ) 
 GEOMETRIC_REPRESENTATION_ITEM ( )  RATIONAL_B_SPLINE_SURFACE ( (
 ( 1.000000000000000000, 0.8660254037844387076, 1.000000000000000000, 0.8660254037844387076, 1.000000000000000000, 0.8660254037844387076, 1.000000000000000000, 0.8660254037844387076, 1.000000000000000000, 0.8660254037844387076, 1.000000000000000000, 0.8660254037844387076, 1.000000000000000000, 0.8660254037844387076, 1.000000000000000000, 0.8660254037844387076, 1.000000000000000000, 0.8660254037844387076, 1.000000000000000000, 0.8660254037844387076, 1.000000000000000000, 0.8660254037844387076, 1.000000000000000000, 0.8660254037844387076, 1.000000000000000000, 0.8660254037844387076, 1.000000000000000000, 0.8660254037844387076, 1.000000000000000000, 0.8660254037844387076, 1.000000000000000000, 0.8660254037844387076, 1.000000000000000000, 0.8660254037844387076, 1.000000000000000000, 0.8660254037844387076, 1.000000000000000000, 0.8660254037844387076, 1.000000000000000000, 0.8660254037844387076, 1.000000000000000000, 0.8660254037844387076, 1.000000000000000000, 0.8660254037844387076, 1.000000000000000000, 0.8660254037844387076, 1.000000000000000000, 0.8660254037844387076, 1.000000000000000000, 0.8660254037844387076, 1.000000000000000000, 0.8660254037844387076, 1.000000000000000000, 0.8660254037844387076, 1.000000000000000000, 0.8660254037844387076, 1.000000000000000000, 0.8660254037844387076, 1.000000000000000000, 0.8660254037844387076, 1.000000000000000000, 0.8660254037844387076, 1.000000000000000000, 0.8660254037844387076, 1.000000000000000000, 0.8660254037844387076, 1.000000000000000000, 0.8660254037844387076, 1.000000000000000000, 0.8660254037844387076, 1.000000000000000000, 0.8660254037844387076, 1.000000000000000000, 0.8660254037844387076, 1.000000000000000000, 0.8660254037844387076, 1.000000000000000000, 0.8660254037844387076, 1.000000000000000000, 0.8660254037844387076, 1.000000000000000000, 0.8660254037844387076, 1.000000000000000000, 0.8660254037844387076, 1.000000000000000000, 0.8660254037844387076, 1.000000000000000000, 0.8660254037844387076, 1.000000000000000000, 0.8660254037844387076, 1.000000000000000000, 0.8660254037844387076, 1.000000000000000000, 0.8660254037844387076, 1.000000000000000000, 0.8660254037844387076, 1.000000000000000000, 0.8660254037844387076, 1.000000000000000000, 0.8660254037844387076, 1.000000000000000000, 0.8660254037844387076, 1.000000000000000000, 0.8660254037844387076, 1.000000000000000000, 0.8660254037844387076, 1.000000000000000000, 0.8660254037844387076, 1.000000000000000000, 0.8660254037844387076, 1.000000000000000000, 0.8660254037844387076, 1.000000000000000000, 0.8660254037844387076, 1.000000000000000000, 0.8660254037844387076, 1.000000000000000000, 0.8660254037844387076, 1.000000000000000000, 0.8660254037844387076, 1.000000000000000000, 0.8660254037844387076, 1.000000000000000000, 0.8660254037844387076, 1.000000000000000000, 0.8660254037844387076, 1.000000000000000000, 0.8660254037844387076, 1.000000000000000000, 0.8660254037844387076, 1.000000000000000000, 0.8660254037844387076, 1.000000000000000000, 0.9111410165655264848, 0.9401539157124900736, 0.9401539157124900736, 0.9401539157124900736),
 ( 1.000000000000000000, 0.8660254037844387076, 1.000000000000000000, 0.8660254037844387076, 1.000000000000000000, 0.8660254037844387076, 1.000000000000000000, 0.8660254037844387076, 1.000000000000000000, 0.8660254037844387076, 1.000000000000000000, 0.8660254037844387076, 1.000000000000000000, 0.8660254037844387076, 1.000000000000000000, 0.8660254037844387076, 1.000000000000000000, 0.8660254037844387076, 1.000000000000000000, 0.8660254037844387076, 1.000000000000000000, 0.8660254037844387076, 1.000000000000000000, 0.8660254037844387076, 1.000000000000000000, 0.8660254037844387076, 1.000000000000000000, 0.8660254037844387076, 1.000000000000000000, 0.8660254037844387076, 1.000000000000000000, 0.8660254037844387076, 1.000000000000000000, 0.8660254037844387076, 1.000000000000000000, 0.8660254037844387076, 1.000000000000000000, 0.8660254037844387076, 1.000000000000000000, 0.8660254037844387076, 1.000000000000000000, 0.8660254037844387076, 1.000000000000000000, 0.8660254037844387076, 1.000000000000000000, 0.8660254037844387076, 1.000000000000000000, 0.8660254037844387076, 1.000000000000000000, 0.8660254037844387076, 1.000000000000000000, 0.8660254037844387076, 1.000000000000000000, 0.8660254037844387076, 1.000000000000000000, 0.8660254037844387076, 1.000000000000000000, 0.8660254037844387076, 1.000000000000000000, 0.8660254037844387076, 1.000000000000000000, 0.8660254037844387076, 1.000000000000000000, 0.8660254037844387076, 1.000000000000000000, 0.8660254037844387076, 1.000000000000000000, 0.8660254037844387076, 1.000000000000000000, 0.8660254037844387076, 1.000000000000000000, 0.8660254037844387076, 1.000000000000000000, 0.8660254037844387076, 1.000000000000000000, 0.8660254037844387076, 1.000000000000000000, 0.8660254037844387076, 1.000000000000000000, 0.8660254037844387076, 1.000000000000000000, 0.8660254037844387076, 1.000000000000000000, 0.8660254037844387076, 1.000000000000000000, 0.8660254037844387076, 1.000000000000000000, 0.8660254037844387076, 1.000000000000000000, 0.8660254037844387076, 1.000000000000000000, 0.8660254037844387076, 1.000000000000000000, 0.8660254037844387076, 1.000000000000000000, 0.8660254037844387076, 1.000000000000000000, 0.8660254037844387076, 1.000000000000000000, 0.8660254037844387076, 1.000000000000000000, 0.8660254037844387076, 1.000000000000000000, 0.8660254037844387076, 1.000000000000000000, 0.8660254037844387076, 1.000000000000000000, 0.8660254037844387076, 1.000000000000000000, 0.8660254037844387076, 1.000000000000000000, 0.8660254037844387076, 1.000000000000000000, 0.8660254037844387076, 1.000000000000000000, 0.8660254037844387076, 1.000000000000000000, 0.8660254037844387076, 1.000000000000000000, 0.8660254037844387076, 1.000000000000000000, 0.8660254037844387076, 1.000000000000000000, 0.8660254037844387076, 1.000000000000000000, 0.8660254037844387076, 1.000000000000000000, 0.8660254037844387076, 1.000000000000000000, 0.8660254037844387076, 1.000000000000000000, 0.8660254037844387076, 1.000000000000000000, 0.9111410165655264848, 0.9401539157124900736, 0.9401539157124900736, 0.9401539157124900736) ) ) 
 REPRESENTATION_ITEM ( '' )  SURFACE ( )  );
#8148 = CARTESIAN_POINT ( 'NONE',  ( 111.5000000000000142, 12.69999999999998508, 30.20101012677667285 ) ) ;
#8149 = CARTESIAN_POINT ( 'NONE',  ( 79.64356964375001269, -32.12812499938548427, 101.5914258081833879 ) ) ;
#8150 = EDGE_CURVE ( 'NONE', #6852, #12897, #6660, .T. ) ;
#8151 = CARTESIAN_POINT ( 'NONE',  ( 82.40000000000001990, -32.53124999877097423, -103.0000000000000000 ) ) ;
#8152 = CARTESIAN_POINT ( 'NONE',  ( -82.39999999999999147, -34.64062499938548711, 103.1828516163667899 ) ) ;
#8153 = CARTESIAN_POINT ( 'NONE',  ( 81.68701737470171054, -32.00000000000000000, 97.18802777794500969 ) ) ;
#8154 = CARTESIAN_POINT ( 'NONE',  ( 82.39999999999999147, -31.60312499938548569, 103.1828516163667899 ) ) ;
#8155 = EDGE_CURVE ( 'NONE', #18433, #729, #2216, .T. ) ;
#8156 = ADVANCED_FACE ( 'NONE', ( #2125 ), #5154, .T. ) ;
#8157 = B_SPLINE_CURVE_WITH_KNOTS ( 'NONE', 3,
 ( #16974, #1241, #8372, #11685, #18837, #7193 ),
 .UNSPECIFIED., .F., .F.,
 ( 4, 2, 4 ),
 ( 0.003805861006858102854, 0.004828937052660004989, 0.005852013098461907557 ),
 .UNSPECIFIED. ) ;
#8158 = CARTESIAN_POINT ( 'NONE',  ( 81.02178482187500208, -31.00312499938548783, -102.3871387122750889 ) ) ;
#8159 = CARTESIAN_POINT ( 'NONE',  ( 231.2217848218749339, -32.01562499938548001, -52.38713871227520968 ) ) ;
#8160 = CARTESIAN_POINT ( 'NONE',  ( -82.39999999999999147, -33.96562499938548285, 96.81714838363319586 ) ) ;
#8161 = CARTESIAN_POINT ( 'NONE',  ( -85.15643035624999868, -31.45312499938548356, -98.40857419181659793 ) ) ;
#8162 = ORIENTED_EDGE ( 'NONE', *, *, #19285, .T. ) ;
#8163 = CARTESIAN_POINT ( 'NONE',  ( 83.77821517812500929, -33.47812499938548569, 102.3871387122750889 ) ) ;
#8164 = CARTESIAN_POINT ( 'NONE',  ( 232.5999999999999375, -34.16249999999999432, 96.99999999999997158 ) ) ;
#8165 = CARTESIAN_POINT ( 'NONE',  ( -81.02178482187500208, -30.89062499938548711, 102.3871387122750889 ) ) ;
#8166 = CARTESIAN_POINT ( 'NONE',  ( -79.64356964375001269, -33.21562499938548996, 101.5914258081833879 ) ) ;
#8167 = CARTESIAN_POINT ( 'NONE',  ( -83.20384757729335945, -31.44240381056766864, 97.00000000000000000 ) ) ;
#8168 = EDGE_LOOP ( 'NONE', ( #10113, #8194, #8790, #17680 ) ) ;
#8169 = CARTESIAN_POINT ( 'NONE',  ( -83.90000000000000568, -34.57500000000000284, -102.5980762113533018 ) ) ;
#8170 = EDGE_CURVE ( 'NONE', #5045, #10401, #10881, .T. ) ;
#8171 = LINE ( 'NONE', #4962, #10360 ) ;
#8172 = CARTESIAN_POINT ( 'NONE',  ( 83.04276107155152431, -34.99999999999999289, -97.06242906295997841 ) ) ;
#8173 = CARTESIAN_POINT ( 'NONE',  ( -79.39999999999999147, -32.86874999877097281, 99.99999999999998579 ) ) ;
#8174 = EDGE_CURVE ( 'NONE', #12416, #13022, #4460, .T. ) ;
#8175 = EDGE_CURVE ( 'NONE', #7020, #13374, #383, .T. ) ;
#8176 = CARTESIAN_POINT ( 'NONE',  ( 232.5999999999999375, -31.37812499938547717, 103.1828516163667899 ) ) ;
#8177 = CARTESIAN_POINT ( 'NONE',  ( -83.90000000000000568, -34.37268749875867968, 102.5980762113533018 ) ) ;
#8178 = CARTESIAN_POINT ( 'NONE',  ( -85.15643035625001289, -35.20312499938548711, 99.99999999999998579 ) ) ;
#8179 = DIRECTION ( 'NONE',  ( 0.5000000000000013323, -0.8660254037844379305, 0.000000000000000000 ) ) ;
#8180 = CARTESIAN_POINT ( 'NONE',  ( -82.40000000000001990, -33.26250000000000284, 97.00000000000000000 ) ) ;
#8181 = CARTESIAN_POINT ( 'NONE',  ( 81.02178482187500208, -31.00312499938548783, 97.61286128772489690 ) ) ;
#8182 = CARTESIAN_POINT ( 'NONE',  ( 83.20384757729337366, -32.79240381056766296, -97.00000000000000000 ) ) ;
#8183 = CARTESIAN_POINT ( 'NONE',  ( 79.64356964374999848, -31.82812499938548356, -99.99999999999998579 ) ) ;
#8184 = LINE ( 'NONE', #11009, #18649 ) ;
#8185 = AXIS2_PLACEMENT_3D ( 'NONE', #14750, #13283, #5874 ) ;
#8186 = EDGE_LOOP ( 'NONE', ( #11019, #1207, #8081, #5748 ) ) ;
#8187 = CARTESIAN_POINT ( 'NONE',  ( 233.9782151781249411, -34.90312499938547575, -52.38713871227520968 ) ) ;
#8188 = CONTEXT_DEPENDENT_SHAPE_REPRESENTATION ( #2845, #9828 ) ;
#8189 = CARTESIAN_POINT ( 'NONE',  ( 235.3564303562499447, -33.66562499938548569, 101.5914258081833879 ) ) ;
#8190 = CARTESIAN_POINT ( 'NONE',  ( 229.8435696437499871, -33.44062499938547717, -51.59142580818350865 ) ) ;
#8191 = B_SPLINE_CURVE_WITH_KNOTS ( 'NONE', 3,
 ( #3561, #3460, #18229, #18326, #9419, #5133, #2195, #8057, #8153, #18418, #1900, #12641, #9717, #741, #18615, #7862, #4943, #838 ),
 .UNSPECIFIED., .F., .F.,
 ( 4, 2, 2, 2, 2, 2, 2, 2, 4 ),
 ( 0.000000000000000000, 0.0007106627595359841631, 0.001421325519071968326, 0.002131988278607952272, 0.002842651038143936652, 0.003553313797679921032, 0.004263976557215904545, 0.004974639316751888925, 0.005685302076287873305 ),
 .UNSPECIFIED. ) ;
#8192 = CARTESIAN_POINT ( 'NONE',  ( -79.64356964375001269, -34.37812499938548427, 98.40857419181659793 ) ) ;
#8193 = CARTESIAN_POINT ( 'NONE',  ( 229.5999999999999375, -32.73749999999999716, -51.73205080756898866 ) ) ;
#8194 = ORIENTED_EDGE ( 'NONE', *, *, #13730, .F. ) ;
#8195 = ORIENTED_EDGE ( 'NONE', *, *, #10124, .T. ) ;
#8196 = CARTESIAN_POINT ( 'NONE',  ( -83.77821517812500929, -31.56562499938548427, -102.3871387122750889 ) ) ;
#8197 = DIRECTION ( 'NONE',  ( 1.000000000000000000, 0.000000000000000000, 0.000000000000000000 ) ) ;
#8198 = ORIENTED_EDGE ( 'NONE', *, *, #9468, .F. ) ;
#8199 = CARTESIAN_POINT ( 'NONE',  ( 81.02178482187500208, -33.70312499938548711, 97.61286128772489690 ) ) ;
#8200 = CARTESIAN_POINT ( 'NONE',  ( -85.40000000000000568, -33.99374999877097281, -99.99999999999998579 ) ) ;
#8201 = CARTESIAN_POINT ( 'NONE',  ( 80.90000000000000568, -33.30000000000000426, 102.5980762113533018 ) ) ;
#8202 = CARTESIAN_POINT ( 'NONE',  ( 231.2217848218749339, -30.62812499938548072, 102.3871387122750889 ) ) ;
#8203 = CARTESIAN_POINT ( 'NONE',  ( -79.39999999999999147, -33.31874999877096855, 99.99999999999998579 ) ) ;
#8204 = EDGE_CURVE ( 'NONE', #2256, #5463, #9513, .T. ) ;
#8205 = EDGE_CURVE ( 'NONE', #3020, #2658, #16781, .T. ) ;
#8206 = CARTESIAN_POINT ( 'NONE',  ( -82.39999999999999147, -34.33124999877097139, 103.4641016151377499 ) ) ;
#8207 = CARTESIAN_POINT ( 'NONE',  ( 84.25709831969352592, -34.99999999999999289, -102.1174602701827752 ) ) ;
#8208 = CARTESIAN_POINT ( 'NONE',  ( 111.0000000000000000, 10.19999999999997620, -139.9999999999999716 ) ) ;
#8209 = DIRECTION ( 'NONE',  ( 1.000000000000000000, -2.001604010742470847E-15, 0.000000000000000000 ) ) ;
#8210 = CARTESIAN_POINT ( 'NONE',  ( 231.2217848218749339, -34.26562499938548001, 97.61286128772489690 ) ) ;
#8211 = ORIENTED_EDGE ( 'NONE', *, *, #14832, .T. ) ;
#8212 =( REPRESENTATION_RELATIONSHIP ('NONE','NONE', #14468, #406 ) REPRESENTATION_RELATIONSHIP_WITH_TRANSFORMATION ( #11109 )SHAPE_REPRESENTATION_RELATIONSHIP( ) );
#8213 = CARTESIAN_POINT ( 'NONE',  ( 83.77821517812500929, -33.81562499938548427, -97.61286128772489690 ) ) ;
#8214 = SURFACE_SIDE_STYLE ('',( #5487 ) ) ;
#8215 = EDGE_CURVE ( 'NONE', #5767, #12372, #14036, .T. ) ;
#8216 = CARTESIAN_POINT ( 'NONE',  ( 232.5999999999999375, -30.50624999877096144, 96.53589838486223584 ) ) ;
#8217 = CARTESIAN_POINT ( 'NONE',  ( 232.5999999999999375, -31.63124999877096144, -46.53589838486234953 ) ) ;
#8218 = VECTOR ( 'NONE', #17742, 1000.000000000000000 ) ;
#8219 = ORIENTED_EDGE ( 'NONE', *, *, #5596, .T. ) ;
#8220 = CARTESIAN_POINT ( 'NONE',  ( 229.5999999999999375, -34.49999999999999289, 99.99999999999998579 ) ) ;
#8221 = CARTESIAN_POINT ( 'NONE',  ( 0.000000000000000000, 0.000000000000000000, -4.484454397937119197 ) ) ;
#8222 = CARTESIAN_POINT ( 'NONE',  ( 3.951447005078451813, 3.704664227300101143, 0.5833333333333334814 ) ) ;
#8223 = ORIENTED_EDGE ( 'NONE', *, *, #13405, .T. ) ;
#8224 = DIRECTION ( 'NONE',  ( 0.000000000000000000, 0.000000000000000000, 1.000000000000000000 ) ) ;
#8225 = ORIENTED_EDGE ( 'NONE', *, *, #16083, .F. ) ;
#8226 = CARTESIAN_POINT ( 'NONE',  ( 232.5999999999999375, -34.16249999999999432, -53.00000000000010658 ) ) ;
#8227 = CARTESIAN_POINT ( 'NONE',  ( 82.39999999999999147, -33.71249999999999858, -96.53589838486223584 ) ) ;
#8228 = CYLINDRICAL_SURFACE ( 'NONE', #5191, 3.000000000000009770 ) ;
#8229 = CARTESIAN_POINT ( 'NONE',  ( -79.39999999999999147, -34.18124999877097281, 98.26794919243110371 ) ) ;
#8230 = CARTESIAN_POINT ( 'NONE',  ( -82.39999999999999147, -34.15856250001229455, 96.53589838486223584 ) ) ;
#8231 = CARTESIAN_POINT ( 'NONE',  ( 0.3126073911696399255, 2.020725942163686728, -3.499999999999999556 ) ) ;
#8232 = CARTESIAN_POINT ( 'NONE',  ( 232.5999999999999375, -33.26249999999999574, 97.00000000000000000 ) ) ;
#8233 = CARTESIAN_POINT ( 'NONE',  ( 79.64356964374999848, -34.98839802032723867, -100.4359666841259440 ) ) ;
#8234 = CARTESIAN_POINT ( 'NONE',  ( -79.39999999999999147, -33.33749999999999858, 98.26794919243110371 ) ) ;
#8235 = CARTESIAN_POINT ( 'NONE',  ( -85.15643035625001289, -32.84062499938548285, 99.99999999999998579 ) ) ;
#8236 = FACE_OUTER_BOUND ( 'NONE', #17718, .T. ) ;
#8237 = ORIENTED_EDGE ( 'NONE', *, *, #3625, .F. ) ;
#8238 = CARTESIAN_POINT ( 'NONE',  ( -83.90000000000000568, -34.42500000000000426, 102.5980762113533018 ) ) ;
#8239 = CARTESIAN_POINT ( 'NONE',  ( -0.5469614295416921346, 4.303013824936271270, -3.535263753543735454 ) ) ;
#8240 = CARTESIAN_POINT ( 'NONE',  ( 229.8435696437499303, -32.02817623523064583, 101.0587761908871443 ) ) ;
#8241 = CARTESIAN_POINT ( 'NONE',  ( -79.64356964375001269, -34.94062499938549138, 98.40857419181659793 ) ) ;
#8242 = CARTESIAN_POINT ( 'NONE',  ( 233.9782151781249411, -34.45312499938548001, -52.38713871227520968 ) ) ;
#8243 = ORIENTED_EDGE ( 'NONE', *, *, #17556, .F. ) ;
#8244 = CARTESIAN_POINT ( 'NONE',  ( 4.086376210449952140, 2.103254844323303008, 3.500000000000000000 ) ) ;
#8245 = CARTESIAN_POINT ( 'NONE',  ( 234.0999999999999375, -33.74999999999999289, -52.59807621135342970 ) ) ;
#8246 = CARTESIAN_POINT ( 'NONE',  ( 82.39999999999999147, -33.62812499938549138, 96.81714838363319586 ) ) ;
#8247 = EDGE_CURVE ( 'NONE', #14672, #4832, #11518, .T. ) ;
#8248 = CARTESIAN_POINT ( 'NONE',  ( 0.02511973781850649831, -4.877415612947427981, -3.751298745799844792 ) ) ;
#8249 = CARTESIAN_POINT ( 'NONE',  ( 235.3564303562499447, -33.02812499938547575, -51.59142580818350154 ) ) ;
#8250 = CARTESIAN_POINT ( 'NONE',  ( -81.02178482187500208, -32.80312499938548854, 102.3871387122750889 ) ) ;
#8251 = CARTESIAN_POINT ( 'NONE',  ( 3.973110223767137850, 2.263313079739336463E-11, 3.565797985667434222 ) ) ;
#8252 = CARTESIAN_POINT ( 'NONE',  ( 79.64356964375001269, -31.22812499938548925, 101.5914258081833879 ) ) ;
#8253 = CARTESIAN_POINT ( 'NONE',  ( 79.64356964375001269, -34.49062499938548854, -98.40857419181659793 ) ) ;
#8254 = CARTESIAN_POINT ( 'NONE',  ( 229.8435696437499871, -32.80312499938548143, -48.40857419181671162 ) ) ;
#8255 = CARTESIAN_POINT ( 'NONE',  ( 25.60000000000000142, 0.000000000000000000, 2.055000000000000160 ) ) ;
#8256 = VERTEX_POINT ( 'NONE', #18349 ) ;
#8257 = CARTESIAN_POINT ( 'NONE',  ( 81.02178482187500208, -33.70312499938548711, 97.61286128772489690 ) ) ;
#8258 = CARTESIAN_POINT ( 'NONE',  ( 1.257172072275274388, -3.892973519170983110, -3.433252694550781303 ) ) ;
#8259 = CARTESIAN_POINT ( 'NONE',  ( -79.39999999999999147, -34.23750000000000426, 98.26794919243110371 ) ) ;
#8260 =( BOUNDED_CURVE ( )  B_SPLINE_CURVE ( 2, ( #5476, #17191, #8390, #4090, #5664, #8295, #9764, #17481, #15821 ),
 .UNSPECIFIED., .F., .F. ) 
 B_SPLINE_CURVE_WITH_KNOTS ( ( 3, 2, 2, 2, 3 ),
 ( 0.8125000000000000000, 0.8194444444444444198, 0.8333333333333333703, 0.8472222222222222099, 0.8541666666666665186 ),
 .UNSPECIFIED. ) 
 CURVE ( )  GEOMETRIC_REPRESENTATION_ITEM ( )  RATIONAL_B_SPLINE_CURVE ( ( 0.9330127018922194093, 0.9330127018922194093, 1.000000000000000000, 0.8660254037844387076, 1.000000000000000000, 0.8660254037844387076, 1.000000000000000000, 0.9330127018922209636, 0.9330127018922194093 ) ) 
 REPRESENTATION_ITEM ( '' )  );
#8261 = DIRECTION ( 'NONE',  ( 0.000000000000000000, 0.000000000000000000, 1.000000000000000000 ) ) ;
#8262 = CARTESIAN_POINT ( 'NONE',  ( -83.77821517812500929, -33.92812499938548854, 97.61286128772489690 ) ) ;
#8263 = CARTESIAN_POINT ( 'NONE',  ( 0.000000000000000000, 0.000000000000000000, -0.3080913168122742518 ) ) ;
#8264 = ORIENTED_EDGE ( 'NONE', *, *, #6247, .T. ) ;
#8265 = CARTESIAN_POINT ( 'NONE',  ( -80.90000000000000568, -33.30000000000000426, -102.5980762113533018 ) ) ;
#8266 = EDGE_CURVE ( 'NONE', #11600, #7637, #13508, .T. ) ;
#8267 = CARTESIAN_POINT ( 'NONE',  ( 0.6937372685066666156, -4.453844082567737672, -3.610536846335894445 ) ) ;
#8268 = CARTESIAN_POINT ( 'NONE',  ( -82.39999999999999147, -30.78356250001229455, 103.4641016151377499 ) ) ;
#8269 = CARTESIAN_POINT ( 'NONE',  ( -83.90000000000000568, -34.07268749875867542, 97.40192378864668399 ) ) ;
#8270 = CARTESIAN_POINT ( 'NONE',  ( -84.57144699476174310, -35.00000000000000000, 97.92073041325134852 ) ) ;
#8271 = CARTESIAN_POINT ( 'NONE',  ( 235.5999999999999943, -32.96249999999999858, 101.7320508075688537 ) ) ;
#8272 = DIRECTION ( 'NONE',  ( 1.000000000000000000, -1.586032892321652482E-15, 0.000000000000000000 ) ) ;
#8273 = CARTESIAN_POINT ( 'NONE',  ( 83.77821517812500929, -30.62812499938548783, 97.61286128772489690 ) ) ;
#8274 = CARTESIAN_POINT ( 'NONE',  ( 235.2013144571816099, -31.99999999999998579, 98.52838665780598149 ) ) ;
#8275 = CARTESIAN_POINT ( 'NONE',  ( -82.39999999999999147, -32.81250000000000000, -103.0000000000000000 ) ) ;
#8276 = CARTESIAN_POINT ( 'NONE',  ( 81.02178482187500208, -32.20312499938548711, -97.61286128772489690 ) ) ;
#8277 = CARTESIAN_POINT ( 'NONE',  ( -82.40000000000000568, -30.00000000000000355, -96.99999999999998579 ) ) ;
#8278 = CIRCLE ( 'NONE', #17335, 2.199999999999993516 ) ;
#8279 = EDGE_CURVE ( 'NONE', #3211, #5198, #2691, .T. ) ;
#8280 = ORIENTED_EDGE ( 'NONE', *, *, #1156, .T. ) ;
#8281 = CARTESIAN_POINT ( 'NONE',  ( 83.90000000000000568, -31.21874999877097068, 97.40192378864668399 ) ) ;
#8282 = CARTESIAN_POINT ( 'NONE',  ( 232.5999999999999375, -34.19062499938547717, 103.1828516163667899 ) ) ;
#8283 = CARTESIAN_POINT ( 'NONE',  ( 232.5999999999999375, -34.19062499938547717, -46.81714838363331666 ) ) ;
#8284 = CARTESIAN_POINT ( 'NONE',  ( -83.77821517812500929, -32.91562499938547859, 97.61286128772489690 ) ) ;
#8285 = CARTESIAN_POINT ( 'NONE',  ( -83.43443729601585801, -35.00000000000000000, -97.42249611015782307 ) ) ;
#8286 = ORIENTED_EDGE ( 'NONE', *, *, #5566, .F. ) ;
#8287 = CARTESIAN_POINT ( 'NONE',  ( -81.02178482187500208, -30.74062499938548498, -102.3871387122750889 ) ) ;
#8288 = CARTESIAN_POINT ( 'NONE',  ( 3.973110223767137850, -2.261515145575163828E-11, -3.565797985667433778 ) ) ;
#8289 = EDGE_CURVE ( 'NONE', #12671, #5588, #2160, .T. ) ;
#8290 = ORIENTED_EDGE ( 'NONE', *, *, #1284, .F. ) ;
#8291 = CARTESIAN_POINT ( 'NONE',  ( 82.39999999999999147, -34.41562499938548569, 103.1828516163667899 ) ) ;
#8292 = CARTESIAN_POINT ( 'NONE',  ( -85.15643035624999868, -31.11562499938548854, -98.40857419181659793 ) ) ;
#8293 = CIRCLE ( 'NONE', #17029, 2.199999999999993516 ) ;
#8294 = CARTESIAN_POINT ( 'NONE',  ( 83.90000000000000568, -33.97500000000000853, 97.40192378864668399 ) ) ;
#8295 = CARTESIAN_POINT ( 'NONE',  ( -85.40000000000000568, -34.53750000000000142, 98.26794919243111792 ) ) ;
#8296 = CARTESIAN_POINT ( 'NONE',  ( -79.39999999999999147, -31.93124999877096926, 98.26794919243110371 ) ) ;
#8297 = CARTESIAN_POINT ( 'NONE',  ( -85.15643035625001289, -30.25312499938548783, 99.99999999999998579 ) ) ;
#8298 = FACE_OUTER_BOUND ( 'NONE', #12528, .T. ) ;
#8299 = LINE ( 'NONE', #6748, #3336 ) ;
#8300 = DIRECTION ( 'NONE',  ( 0.000000000000000000, -1.000000000000000000, 0.000000000000000000 ) ) ;
#8301 = CARTESIAN_POINT ( 'NONE',  ( 232.5999999999999375, -32.36249999999999716, 96.53589838486223584 ) ) ;
#8302 = VERTEX_POINT ( 'NONE', #9740 ) ;
#8303 = CARTESIAN_POINT ( 'NONE',  ( 85.15643035625001289, -32.84062499938548285, -99.99999999999998579 ) ) ;
#8304 = CARTESIAN_POINT ( 'NONE',  ( 229.5999999999999375, -30.88124999877096144, 98.26794919243111792 ) ) ;
#8305 = CARTESIAN_POINT ( 'NONE',  ( 234.0999999999999375, -30.54374999877096286, -52.59807621135342970 ) ) ;
#8306 = ORIENTED_EDGE ( 'NONE', *, *, #8667, .F. ) ;
#8307 = AXIS2_PLACEMENT_3D ( 'NONE', #6873, #1007, #8605 ) ;
#8308 = CARTESIAN_POINT ( 'NONE',  ( -84.70833260042415702, -35.00006955123599539, 98.08383195543535749 ) ) ;
#8309 = CARTESIAN_POINT ( 'NONE',  ( 112.9622674055505342, 10.33079765201859779, -149.9987168157428528 ) ) ;
#8310 = CARTESIAN_POINT ( 'NONE',  ( 2.171643655288379993, -3.365003104552334978, -1.195831703456429434E-14 ) ) ;
#8311 = EDGE_LOOP ( 'NONE', ( #2953, #5169, #7270, #7617 ) ) ;
#8312 = CARTESIAN_POINT ( 'NONE',  ( -80.90000000000000568, -32.04374999877096997, 102.5980762113533018 ) ) ;
#8313 = CARTESIAN_POINT ( 'NONE',  ( -82.40000000000000568, -50.00000000000000000, 92.49999999999997158 ) ) ;
#8314 = EDGE_LOOP ( 'NONE', ( #230, #4785, #9051, #18449, #16250 ) ) ;
#8315 =( NAMED_UNIT ( * ) PLANE_ANGLE_UNIT ( ) SI_UNIT ( $, .RADIAN. ) );
#8316 = CARTESIAN_POINT ( 'NONE',  ( 80.90000000000000568, -31.94999999999999929, -97.40192378864668399 ) ) ;
#8317 = CARTESIAN_POINT ( 'NONE',  ( 244.7999999999999545, -34.51168759575591594, -100.0000000000000000 ) ) ;
#8318 = CARTESIAN_POINT ( 'NONE',  ( -81.02178482187500208, -31.45312499938549067, 102.3871387122750889 ) ) ;
#8319 = CARTESIAN_POINT ( 'NONE',  ( -85.40000000000000568, -30.45000000000000284, 99.99999999999998579 ) ) ;
#8320 = EDGE_CURVE ( 'NONE', #4792, #5820, #6160, .T. ) ;
#8321 = LINE ( 'NONE', #11252, #582 ) ;
#8322 = DIRECTION ( 'NONE',  ( -0.000000000000000000, -0.000000000000000000, -1.000000000000000000 ) ) ;
#8323 = CARTESIAN_POINT ( 'NONE',  ( -69.99999999999998579, -32.00000000000000000, -150.0000000000000000 ) ) ;
#8324 = CARTESIAN_POINT ( 'NONE',  ( -82.39999999999999147, -32.05312499938548854, 96.81714838363319586 ) ) ;
#8325 = B_SPLINE_CURVE_WITH_KNOTS ( 'NONE', 3,
 ( #13102, #16331, #19072, #1389, #5690, #10174, #11641, #5883, #16138, #2846, #7337, #19265, #7052 ),
 .UNSPECIFIED., .F., .F.,
 ( 4, 3, 3, 3, 4 ),
 ( 1.387778780781445521E-17, 9.843749969274346115E-05, 0.0001968749993854869223, 0.0002955393327547696384, 0.0003942036661240663135 ),
 .UNSPECIFIED. ) ;
#8326 = CARTESIAN_POINT ( 'NONE',  ( -99.99999999999998579, 0.000000000000000000, 150.0000000000000000 ) ) ;
#8327 = ORIENTED_EDGE ( 'NONE', *, *, #6247, .F. ) ;
#8328 = CARTESIAN_POINT ( 'NONE',  ( 79.39999999999999147, -32.96250000000000568, 98.26794919243113213 ) ) ;
#8329 = CARTESIAN_POINT ( 'NONE',  ( 235.0804598586379939, -35.00000000000002132, 98.55723758691048886 ) ) ;
#8330 = CARTESIAN_POINT ( 'NONE',  ( 85.40000000000000568, -34.85624999877096997, 98.26794919243111792 ) ) ;
#8331 = PLANE ( 'NONE',  #9909 ) ;
#8332 = CARTESIAN_POINT ( 'NONE',  ( -79.64356964374999848, -34.97812499938548569, 99.99999999999998579 ) ) ;
#8333 = CARTESIAN_POINT ( 'NONE',  ( 235.3564303562499447, -31.30312499938547788, -48.40857419181671162 ) ) ;
#8334 = ORIENTED_EDGE ( 'NONE', *, *, #3381, .F. ) ;
#8335 = ADVANCED_FACE ( 'NONE', ( #5641 ), #859, .F. ) ;
#8336 = CARTESIAN_POINT ( 'NONE',  ( 4.055498735588686010, -1.410041617599707475, 3.568038744583201805 ) ) ;
#8337 = CARTESIAN_POINT ( 'NONE',  ( -85.15643035624999868, -35.11426541925033007, 98.99674735228809652 ) ) ;
#8338 = CARTESIAN_POINT ( 'NONE',  ( -83.90000000000000568, -30.46874999877096712, 97.40192378864668399 ) ) ;
#8339 = CARTESIAN_POINT ( 'NONE',  ( 79.64356964374999848, -32.16562499938548569, 99.99999999999998579 ) ) ;
#8340 = COLOUR_RGB ( '',0.8941176470588234615, 0.8941176470588234615, 0.8941176470588234615 ) ;
#8341 = CARTESIAN_POINT ( 'NONE',  ( 82.40000000000000568, -31.99999999999999289, 99.99999999999998579 ) ) ;
#8342 = CARTESIAN_POINT ( 'NONE',  ( 229.8435696437499303, -32.39062499938548001, -50.00000000000011369 ) ) ;
#8343 = CARTESIAN_POINT ( 'NONE',  ( -85.15643035625001289, -32.99062499938548854, 98.40857419181659793 ) ) ;
#8344 = CIRCLE ( 'NONE', #13948, 0.5155456020628804703 ) ;
#8345 = CARTESIAN_POINT ( 'NONE',  ( -81.02178482187500208, -33.25312499938548427, -97.61286128772489690 ) ) ;
#8346 = CARTESIAN_POINT ( 'NONE',  ( 82.39999999999999147, -32.05312499938548854, 103.1828516163667899 ) ) ;
#8347 = COLOUR_RGB ( '',0.8941176470588234615, 0.8941176470588234615, 0.8941176470588234615 ) ;
#8348 = CARTESIAN_POINT ( 'NONE',  ( 82.39999999999999147, -33.96562499938548285, -96.81714838363319586 ) ) ;
#8349 = CARTESIAN_POINT ( 'NONE',  ( 233.9782151781249411, -33.89062499938548001, -52.38713871227520968 ) ) ;
#8350 = CARTESIAN_POINT ( 'NONE',  ( -85.15643035625001289, -33.29062499938547859, 99.99999999999998579 ) ) ;
#8351 = CARTESIAN_POINT ( 'NONE',  ( 85.15643035624999868, -30.17812499938548498, -98.40857419181659793 ) ) ;
#8352 = ORIENTED_EDGE ( 'NONE', *, *, #4099, .F. ) ;
#8353 = CARTESIAN_POINT ( 'NONE',  ( 79.64356964375001269, -34.56562499938549138, 98.40857419181659793 ) ) ;
#8354 = DIRECTION ( 'NONE',  ( 0.000000000000000000, 0.000000000000000000, 1.000000000000000000 ) ) ;
#8355 = CARTESIAN_POINT ( 'NONE',  ( -79.39999999999999147, -32.96250000000000568, 101.7320508075688537 ) ) ;
#8356 = CARTESIAN_POINT ( 'NONE',  ( -79.64356964375001269, -31.67812499938548143, 98.40857419181659793 ) ) ;
#8357 = CARTESIAN_POINT ( 'NONE',  ( -79.64356964375001269, -31.30312499938548854, 101.5914258081833879 ) ) ;
#8358 = DIRECTION ( 'NONE',  ( -1.000000000000000000, 0.000000000000000000, 0.000000000000000000 ) ) ;
#8359 = EDGE_LOOP ( 'NONE', ( #2628, #12481, #1829, #3429 ) ) ;
#8360 = CARTESIAN_POINT ( 'NONE',  ( -85.40000000000000568, -32.70000000000000284, -99.99999999999998579 ) ) ;
#8361 = CIRCLE ( 'NONE', #19292, 7.000000000000006217 ) ;
#8362 = VECTOR ( 'NONE', #11154, 1000.000000000000000 ) ;
#8363 = CARTESIAN_POINT ( 'NONE',  ( -79.39999999999999147, -32.41874999877096997, 99.99999999999998579 ) ) ;
#8364 = DIRECTION ( 'NONE',  ( 1.000000000000000000, 0.000000000000000000, -0.000000000000000000 ) ) ;
#8365 = CARTESIAN_POINT ( 'NONE',  ( -85.40000000000000568, -29.95276344769438737, 101.9998975609119469 ) ) ;
#8366 = CARTESIAN_POINT ( 'NONE',  ( -80.90000000000000568, -34.80000000000000426, 102.5980762113533018 ) ) ;
#8367 = DIRECTION ( 'NONE',  ( -0.000000000000000000, -1.000000000000000000, -0.000000000000000000 ) ) ;
#8368 = CARTESIAN_POINT ( 'NONE',  ( -83.77821517812500929, -30.51562499938548711, 102.3871387122750889 ) ) ;
#8369 = CARTESIAN_POINT ( 'NONE',  ( -82.40000000000001990, -32.53124999877097423, -97.00000000000000000 ) ) ;
#8370 = CARTESIAN_POINT ( 'NONE',  ( 4.000000000000000888, 1.539600717838996990, -3.300726591567079815 ) ) ;
#8371 = ADVANCED_FACE ( 'NONE', ( #6822 ), #14320, .T. ) ;
#8372 = CARTESIAN_POINT ( 'NONE',  ( 0.1381419387119174058, -1.355287006778759684, 3.500000000000000888 ) ) ;
#8373 = CARTESIAN_POINT ( 'NONE',  ( 82.39999999999999147, -33.06562499938548427, -96.81714838363319586 ) ) ;
#8374 = AXIS2_PLACEMENT_3D ( 'NONE', #16163, #10585, #18401 ) ;
#8375 = CARTESIAN_POINT ( 'NONE',  ( -85.40000000000000568, -33.13124999877096855, 98.26794919243111792 ) ) ;
#8376 = ORIENTED_EDGE ( 'NONE', *, *, #9704, .F. ) ;
#8377 = CARTESIAN_POINT ( 'NONE',  ( 235.2218879900010506, -35.00000000000000000, -49.14934632385183733 ) ) ;
#8378 =( NAMED_UNIT ( * ) SI_UNIT ( $, .STERADIAN. ) SOLID_ANGLE_UNIT ( ) );
#8379 = CARTESIAN_POINT ( 'NONE',  ( 231.2217848218749339, -33.77812499938547575, 102.3871387122750889 ) ) ;
#8380 = CARTESIAN_POINT ( 'NONE',  ( 232.5999999999999375, -32.61562499938548143, -53.18285161636690361 ) ) ;
#8381 = CARTESIAN_POINT ( 'NONE',  ( -85.15643035625001289, -35.09062499938548285, 99.99999999999998579 ) ) ;
#8382 = CARTESIAN_POINT ( 'NONE',  ( -85.10336890117801545, -35.00000000000000711, -99.00607337841718447 ) ) ;
#8383 = VERTEX_POINT ( 'NONE', #7097 ) ;
#8384 = CARTESIAN_POINT ( 'NONE',  ( -79.64356964374999848, -31.71562499938548285, -99.99999999999998579 ) ) ;
#8385 = CARTESIAN_POINT ( 'NONE',  ( -82.40000000000000568, -30.00000000000000355, -103.0000000000000000 ) ) ;
#8386 = ORIENTED_EDGE ( 'NONE', *, *, #7239, .F. ) ;
#8387 = CARTESIAN_POINT ( 'NONE',  ( 81.02178482187500208, -33.55312499938548854, 102.3871387122750889 ) ) ;
#8388 = CARTESIAN_POINT ( 'NONE',  ( -83.77821517812500929, -31.97812499938548925, -97.61286128772489690 ) ) ;
#8389 = CARTESIAN_POINT ( 'NONE',  ( -85.40000000000000568, -30.43124999877096926, -101.7320508075688679 ) ) ;
#8390 = CARTESIAN_POINT ( 'NONE',  ( -83.90000000000000568, -34.42500000000000426, 102.5980762113533018 ) ) ;
#8391 = CARTESIAN_POINT ( 'NONE',  ( -85.40000000000000568, -33.58124999877097139, 98.26794919243111792 ) ) ;
#8392 = CARTESIAN_POINT ( 'NONE',  ( -85.15643035624999868, -30.66562499938548569, 101.5914258081833879 ) ) ;
#8393 = CARTESIAN_POINT ( 'NONE',  ( 232.5999999999999375, -29.99999999999999645, -50.00000000000011369 ) ) ;
#8394 = CARTESIAN_POINT ( 'NONE',  ( -80.90000000000000568, -34.14374999877097139, -102.5980762113533018 ) ) ;
#8395 = DIRECTION ( 'NONE',  ( 1.000000000000000000, 0.000000000000000000, -0.000000000000000000 ) ) ;
#8396 = CARTESIAN_POINT ( 'NONE',  ( 229.5999999999999375, -30.48749999999999005, 98.26794919243111792 ) ) ;
#8397 = EDGE_CURVE ( 'NONE', #6950, #518, #15799, .T. ) ;
#8398 = ORIENTED_EDGE ( 'NONE', *, *, #6894, .F. ) ;
#8399 = CARTESIAN_POINT ( 'NONE',  ( 79.64356964374998427, -33.02812499938548285, -98.40857419181659793 ) ) ;
#8400 = CARTESIAN_POINT ( 'NONE',  ( 229.5999999999999375, -33.05624999877096570, 101.7320508075688679 ) ) ;
#8401 = CARTESIAN_POINT ( 'NONE',  ( 234.0999999999999375, -31.89374999877096073, -52.59807621135342970 ) ) ;
#8402 = ORIENTED_EDGE ( 'NONE', *, *, #13303, .T. ) ;
#8403 = CARTESIAN_POINT ( 'NONE',  ( -82.39999999999999147, -35.23124999877096997, 103.4641016151377499 ) ) ;
#8404 = CARTESIAN_POINT ( 'NONE',  ( -79.64356964374998427, -31.67812499938548143, 98.40857419181659793 ) ) ;
#8405 = CYLINDRICAL_SURFACE ( 'NONE', #18484, 3.000000000000002665 ) ;
#8406 = ORIENTED_EDGE ( 'NONE', *, *, #9187, .T. ) ;
#8407 = CARTESIAN_POINT ( 'NONE',  ( 4.158806965674310518, -4.075748668183989842, -0.05940377217584014852 ) ) ;
#8408 = CARTESIAN_POINT ( 'NONE',  ( 231.0999999999999375, -33.01874999877096428, 102.5980762113533018 ) ) ;
#8409 = ORIENTED_EDGE ( 'NONE', *, *, #1500, .T. ) ;
#8410 = CARTESIAN_POINT ( 'NONE',  ( -80.90000000000000568, -32.10000000000000142, -97.40192378864668399 ) ) ;
#8411 = CARTESIAN_POINT ( 'NONE',  ( 83.90000000000000568, -33.52499999999999858, -102.5980762113533018 ) ) ;
#8412 = CARTESIAN_POINT ( 'NONE',  ( 1.562775787684183633E-16, 0.3423821193476820346, 3.500000000000000000 ) ) ;
#8413 = EDGE_CURVE ( 'NONE', #19103, #4556, #14411, .T. ) ;
#8414 = CARTESIAN_POINT ( 'NONE',  ( -83.77821517812500929, -31.97812499938548925, 102.3871387122750889 ) ) ;
#8415 = CARTESIAN_POINT ( 'NONE',  ( -80.90000000000000568, -32.55000000000000426, 102.5980762113533018 ) ) ;
#8416 = CARTESIAN_POINT ( 'NONE',  ( -82.40000000000000568, -34.61250000000001137, -102.9999999999999858 ) ) ;
#8417 = ADVANCED_FACE ( 'NONE', ( #6914 ), #8147, .T. ) ;
#8418 = CARTESIAN_POINT ( 'NONE',  ( 94.79999999999995453, -32.00000000000000000, -150.0000000000000000 ) ) ;
#8419 = CARTESIAN_POINT ( 'NONE',  ( 84.85538848574883275, -34.99999999999999289, 101.7224313860079263 ) ) ;
#8420 = CARTESIAN_POINT ( 'NONE',  ( -82.40000000000001990, -33.20624999877097849, 97.00000000000000000 ) ) ;
#8421 = ORIENTED_EDGE ( 'NONE', *, *, #7384, .F. ) ;
#8422 = LINE ( 'NONE', #18888, #8039 ) ;
#8423 = LINE ( 'NONE', #1098, #6808 ) ;
#8424 = PRODUCT ( 'hex flange nut gradea_iso_ISO - 4161 - M5 - N', 'hex flange nut gradea_iso_ISO - 4161 - M5 - N', '', ( #12673 ) ) ;
#8425 = DIRECTION ( 'NONE',  ( -0.000000000000000000, -1.000000000000000000, -0.000000000000000000 ) ) ;
#8426 = CARTESIAN_POINT ( 'NONE',  ( 4.000000000000000000, 2.309401076758497151, -3.433295621305379353 ) ) ;
#8427 = CARTESIAN_POINT ( 'NONE',  ( -85.15643035625001289, -34.30312499938548854, 99.99999999999998579 ) ) ;
#8428 = EDGE_CURVE ( 'NONE', #9376, #10447, #16266, .T. ) ;
#8429 = CARTESIAN_POINT ( 'NONE',  ( 232.5999999999999375, -31.60312499938548214, -53.18285161636690361 ) ) ;
#8430 = EDGE_LOOP ( 'NONE', ( #3791, #12729, #15733, #8546, #7327 ) ) ;
#8431 = CARTESIAN_POINT ( 'NONE',  ( -79.64356964375001269, -33.47812499938547859, 98.40857419181659793 ) ) ;
#8432 = CARTESIAN_POINT ( 'NONE',  ( -85.40000000000000568, -30.39374999877097139, 99.99999999999998579 ) ) ;
#8433 = CARTESIAN_POINT ( 'NONE',  ( 81.02178482187500208, -34.34062499938548285, 102.3871387122750889 ) ) ;
#8434 = DIRECTION ( 'NONE',  ( -0.000000000000000000, -1.000000000000000000, -0.000000000000000000 ) ) ;
#8435 = CARTESIAN_POINT ( 'NONE',  ( 110.9999999999999574, -21.80000000000003268, -137.3499999999999943 ) ) ;
#8436 = ADVANCED_FACE ( 'NONE', ( #7371 ), #10145, .F. ) ;
#8437 = CARTESIAN_POINT ( 'NONE',  ( -81.02178482187500208, -34.90312499938548285, 97.61286128772489690 ) ) ;
#8438 = CARTESIAN_POINT ( 'NONE',  ( -85.15643035625001289, -34.26562499938548711, -98.40857419181659793 ) ) ;
#8439 = CARTESIAN_POINT ( 'NONE',  ( 79.64356964375001269, -31.30312499938548854, 98.40857419181659793 ) ) ;
#8440 = CARTESIAN_POINT ( 'NONE',  ( 81.02178482187500208, -34.45312499938548711, -97.61286128772489690 ) ) ;
#8441 = CARTESIAN_POINT ( 'NONE',  ( 232.5999999999999375, -32.95312499938548001, -53.18285161636690361 ) ) ;
#8442 = CARTESIAN_POINT ( 'NONE',  ( -85.15643035625001289, -33.25312499938548427, 101.5914258081833879 ) ) ;
#8443 = CARTESIAN_POINT ( 'NONE',  ( 85.15643035625001289, -31.49062499938548498, -99.99999999999998579 ) ) ;
#8444 = ORIENTED_EDGE ( 'NONE', *, *, #8247, .F. ) ;
#8445 = CARTESIAN_POINT ( 'NONE',  ( 83.77821517812500929, -34.82812499938548711, 102.3871387122750889 ) ) ;
#8446 = CARTESIAN_POINT ( 'NONE',  ( -82.40000000000000568, -34.38749999999999574, -96.99999999999998579 ) ) ;
#8447 = ADVANCED_FACE ( 'NONE', ( #13694 ), #15062, .T. ) ;
#8448 = CARTESIAN_POINT ( 'NONE',  ( -79.39999999999999147, -33.86250000000000426, 101.7320508075688537 ) ) ;
#8449 = CARTESIAN_POINT ( 'NONE',  ( -79.64356964374999848, -32.16562499938548569, 99.99999999999998579 ) ) ;
#8450 = CARTESIAN_POINT ( 'NONE',  ( -82.39999999999999147, -31.82812499938548356, 103.1828516163667899 ) ) ;
#8451 = CARTESIAN_POINT ( 'NONE',  ( -83.20384757729335945, -31.25759618943233775, 102.9999999999999858 ) ) ;
#8452 = CARTESIAN_POINT ( 'NONE',  ( 235.3564303562499447, -32.20312499938548001, 101.5914258081833879 ) ) ;
#8453 = CYLINDRICAL_SURFACE ( 'NONE', #5494, 2.500000000000000444 ) ;
#8454 = CARTESIAN_POINT ( 'NONE',  ( -85.40000000000000568, -30.44606250001229242, 99.99999999999998579 ) ) ;
#8455 = CARTESIAN_POINT ( 'NONE',  ( -79.39999999999999147, -34.76250000000000284, 101.7320508075688537 ) ) ;
#8456 = DIRECTION ( 'NONE',  ( 0.000000000000000000, -1.000000000000000000, 0.000000000000000000 ) ) ;
#8457 = CARTESIAN_POINT ( 'NONE',  ( 235.5999999999999375, -32.92499999999999716, 99.99999999999998579 ) ) ;
#8458 = CARTESIAN_POINT ( 'NONE',  ( -82.39999999999999147, -33.48750000000000426, 103.0000000000000000 ) ) ;
#8459 = CARTESIAN_POINT ( 'NONE',  ( 4.000000000000000000, -2.309401076758514915, -3.433295621305383349 ) ) ;
#8460 = CARTESIAN_POINT ( 'NONE',  ( 246.9999999999999716, -5.000000000000004441, 150.0000000000000000 ) ) ;
#8461 = CARTESIAN_POINT ( 'NONE',  ( -83.90000000000000568, -32.56874999877096855, -97.40192378864668399 ) ) ;
#8462 = CARTESIAN_POINT ( 'NONE',  ( 81.02178482187500208, -33.70312499938548711, -102.3871387122750889 ) ) ;
#8463 = FACE_OUTER_BOUND ( 'NONE', #12711, .T. ) ;
#8464 = VERTEX_POINT ( 'NONE', #9097 ) ;
#8465 = CARTESIAN_POINT ( 'NONE',  ( 82.39999999999999147, -33.43124999877097281, 96.53589838486223584 ) ) ;
#8466 = CARTESIAN_POINT ( 'NONE',  ( 233.2099102960628443, -35.00000000000002842, -47.30603528924583401 ) ) ;
#8467 = CARTESIAN_POINT ( 'NONE',  ( 235.3564303562499447, -32.31562499938547717, -48.40857419181671162 ) ) ;
#8468 = CARTESIAN_POINT ( 'NONE',  ( -85.15643035624999868, -35.11426555956768425, 98.99674139749697588 ) ) ;
#8469 = FACE_OUTER_BOUND ( 'NONE', #12656, .T. ) ;
#8470 = EDGE_LOOP ( 'NONE', ( #7555, #11939, #15269, #1469 ) ) ;
#8471 = CARTESIAN_POINT ( 'NONE',  ( -85.15643035624999868, -34.15312499938548285, -98.40857419181659793 ) ) ;
#8472 = DIRECTION ( 'NONE',  ( -1.000000000000000000, 0.000000000000000000, 0.000000000000000000 ) ) ;
#8473 = ORIENTED_EDGE ( 'NONE', *, *, #3245, .F. ) ;
#8474 = CARTESIAN_POINT ( 'NONE',  ( 81.02178482187500208, -34.15312499938548285, 97.61286128772489690 ) ) ;
#8475 = CARTESIAN_POINT ( 'NONE',  ( -82.39999999999999147, -31.94062499938548427, -96.81714838363319586 ) ) ;
#8476 = CARTESIAN_POINT ( 'NONE',  ( 82.39999999999999147, -33.26250000000000284, 103.4641016151377499 ) ) ;
#8477 = CARTESIAN_POINT ( 'NONE',  ( 82.40000000000001990, -32.08124999877097139, 97.00000000000000000 ) ) ;
#8478 = CARTESIAN_POINT ( 'NONE',  ( -85.40000000000000568, -30.35438844644077605, 101.9998975609119469 ) ) ;
#8479 = CARTESIAN_POINT ( 'NONE',  ( -83.77821517812500929, -30.62812499938548783, 102.3871387122750889 ) ) ;
#8480 = CARTESIAN_POINT ( 'NONE',  ( -81.02178482187500208, -33.44062499938548427, -102.3871387122750889 ) ) ;
#8481 = CIRCLE ( 'NONE', #5696, 3.500000000000000000 ) ;
#8482 =( BOUNDED_CURVE ( )  B_SPLINE_CURVE ( 2, ( #6199, #4829, #13510, #1980, #16449 ),
 .UNSPECIFIED., .F., .F. ) 
 B_SPLINE_CURVE_WITH_KNOTS ( ( 3, 2, 3 ),
 ( 0.2975293541897524041, 0.3055555555555555802, 0.3125000000000001665 ),
 .UNSPECIFIED. ) 
 CURVE ( )  GEOMETRIC_REPRESENTATION_ITEM ( )  RATIONAL_B_SPLINE_CURVE ( ( 0.9346381638529799307, 0.9225778897267649103, 1.000000000000000000, 0.9330127018922177440, 0.9330127018922194093 ) ) 
 REPRESENTATION_ITEM ( '' )  );
#8483 = VECTOR ( 'NONE', #4019, 1000.000000000000000 ) ;
#8484 = DIRECTION ( 'NONE',  ( -1.000000000000000000, 0.000000000000000000, 0.000000000000000000 ) ) ;
#8485 = CARTESIAN_POINT ( 'NONE',  ( 83.90000000000000568, -32.71874999877096712, -97.40192378864668399 ) ) ;
#8486 = CARTESIAN_POINT ( 'NONE',  ( 235.5999999999999943, -31.98749999999999361, 98.26794919243110371 ) ) ;
#8487 = ORIENTED_EDGE ( 'NONE', *, *, #16270, .F. ) ;
#8488 = CARTESIAN_POINT ( 'NONE',  ( 83.77821517812500929, -34.71562499938548285, -97.61286128772489690 ) ) ;
#8489 =( NAMED_UNIT ( * ) SI_UNIT ( $, .STERADIAN. ) SOLID_ANGLE_UNIT ( ) );
#8490 = CARTESIAN_POINT ( 'NONE',  ( 234.0999999999999375, -32.94374999877096144, 102.5980762113533018 ) ) ;
#8491 = CARTESIAN_POINT ( 'NONE',  ( 234.0999999999999375, -31.59374999877096712, -47.40192378864679768 ) ) ;
#8492 = CARTESIAN_POINT ( 'NONE',  ( 231.7961524227065695, -32.55134618820330417, 103.0000000000000000 ) ) ;
#8493 = CARTESIAN_POINT ( 'NONE',  ( -82.39999999999999147, -31.15312499938548640, 96.81714838363319586 ) ) ;
#8494 = ORIENTED_EDGE ( 'NONE', *, *, #4260, .F. ) ;
#8495 = ORIENTED_EDGE ( 'NONE', *, *, #10124, .F. ) ;
#8496 = VECTOR ( 'NONE', #13988, 1000.000000000000000 ) ;
#8497 = AXIS2_PLACEMENT_3D ( 'NONE', #11856, #7364, #7462 ) ;
#8498 = CARTESIAN_POINT ( 'NONE',  ( 235.5999999999999943, -33.73124999877096286, -51.73205080756900287 ) ) ;
#8499 = ORIENTED_EDGE ( 'NONE', *, *, #9274, .T. ) ;
#8500 = CARTESIAN_POINT ( 'NONE',  ( 83.90000000000000568, -33.07500000000000284, -102.5980762113533018 ) ) ;
#8501 = CARTESIAN_POINT ( 'NONE',  ( 5.599999999999999645, -2.020725942163695166, -3.500000000000000000 ) ) ;
#8502 = EDGE_CURVE ( 'NONE', #9169, #3491, #229, .T. ) ;
#8503 = EDGE_CURVE ( 'NONE', #1391, #15492, #2895, .T. ) ;
#8504 = CARTESIAN_POINT ( 'NONE',  ( -81.02178482187500208, -30.85312499938548569, 97.61286128772489690 ) ) ;
#8505 = CARTESIAN_POINT ( 'NONE',  ( -80.90000000000000568, -32.40000000000000568, 97.40192378864668399 ) ) ;
#8506 = LINE ( 'NONE', #14275, #18355 ) ;
#8507 =( LENGTH_UNIT ( ) NAMED_UNIT ( * ) SI_UNIT ( .MILLI., .METRE. ) );
#8508 = CARTESIAN_POINT ( 'NONE',  ( 83.77821517812500929, -34.82812499938548711, -97.61286128772489690 ) ) ;
#8509 = CARTESIAN_POINT ( 'NONE',  ( 80.32125193361331128, -34.99999999999999289, 102.0234471769926472 ) ) ;
#8510 = LINE ( 'NONE', #5691, #9606 ) ;
#8511 = CIRCLE ( 'NONE', #114, 2.500000000000000444 ) ;
#8512 = DIRECTION ( 'NONE',  ( 0.000000000000000000, -1.000000000000000000, 0.000000000000000000 ) ) ;
#8513 = EDGE_LOOP ( 'NONE', ( #16634, #14971, #5979, #6210 ) ) ;
#8514 = CARTESIAN_POINT ( 'NONE',  ( -79.64356964375001269, -34.94062499938549138, -101.5914258081833879 ) ) ;
#8515 = B_SPLINE_CURVE_WITH_KNOTS ( 'NONE', 3,
 ( #18682, #17404, #17209, #14172, #15553, #3722, #9783, #14360, #14076, #9980, #5106, #6863, #15933, #2536, #9880, #15649 ),
 .UNSPECIFIED., .F., .F.,
 ( 4, 3, 3, 3, 3, 4 ),
 ( 0.000000000000000000, 3.315506744709606176E-05, 6.608280158701084731E-05, 0.0001026520855292453537, 0.0001376952025668689477, 0.0001398064759194506818 ),
 .UNSPECIFIED. ) ;
#8516 = LINE ( 'NONE', #17224, #13026 ) ;
#8517 = EDGE_CURVE ( 'NONE', #5861, #9248, #18511, .T. ) ;
#8518 = CARTESIAN_POINT ( 'NONE',  ( -82.40000000000000568, -30.00000000000000355, -99.99999999999998579 ) ) ;
#8519 = CARTESIAN_POINT ( 'NONE',  ( -83.90000000000000568, -34.87500000000000000, -97.40192378864668399 ) ) ;
#8520 = CARTESIAN_POINT ( 'NONE',  ( -79.64356964375001269, -33.66562499938549280, 101.5914258081833879 ) ) ;
#8521 = DIRECTION ( 'NONE',  ( 1.000000000000000000, -0.000000000000000000, -2.407412430484046130E-31 ) ) ;
#8522 = ADVANCED_FACE ( 'NONE', ( #15350 ), #10951, .F. ) ;
#8523 = CARTESIAN_POINT ( 'NONE',  ( 232.5999999999999375, -30.92812499938547433, -46.81714838363331666 ) ) ;
#8524 = B_SPLINE_CURVE_WITH_KNOTS ( 'NONE', 3,
 ( #13474, #307, #6159, #6445, #4987 ),
 .UNSPECIFIED., .F., .F.,
 ( 4, 1, 4 ),
 ( 0.000000000000000000, 0.002020725942163692675, 0.004041451884327385349 ),
 .UNSPECIFIED. ) ;
#8525 = ORIENTED_EDGE ( 'NONE', *, *, #16123, .F. ) ;
#8526 = CARTESIAN_POINT ( 'NONE',  ( -83.77821517812500929, -33.81562499938548427, 97.61286128772489690 ) ) ;
#8527 = CARTESIAN_POINT ( 'NONE',  ( -79.39999999999999147, -30.61874999877096926, 99.99999999999998579 ) ) ;
#8528 = CARTESIAN_POINT ( 'NONE',  ( 83.77821517812500929, -34.71562499938548285, 102.3871387122750889 ) ) ;
#8529 = CARTESIAN_POINT ( 'NONE',  ( -82.40000000000000568, -33.03750000000000142, -96.99999999999998579 ) ) ;
#8530 = CARTESIAN_POINT ( 'NONE',  ( 233.9782151781249411, -30.44062499938548072, 102.3871387122750889 ) ) ;
#8531 = DIRECTION ( 'NONE',  ( -1.000000000000000000, 1.445602896647337931E-15, 0.000000000000000000 ) ) ;
#8532 =( BOUNDED_CURVE ( )  B_SPLINE_CURVE ( 2, ( #13250, #5839, #2276, #17035, #11261, #13802, #445 ),
 .UNSPECIFIED., .F., .F. ) 
 B_SPLINE_CURVE_WITH_KNOTS ( ( 3, 2, 2, 3 ),
 ( 0.8958333333333332593, 0.9027777777777777901, 0.9166666666666666297, 0.9258785066912882389 ),
 .UNSPECIFIED. ) 
 CURVE ( )  GEOMETRIC_REPRESENTATION_ITEM ( )  RATIONAL_B_SPLINE_CURVE ( ( 0.9330127018922192983, 0.9330127018922187432, 1.000000000000000000, 0.8660254037844387076, 1.000000000000000000, 0.9111410165655264848, 0.9401539157124900736 ) ) 
 REPRESENTATION_ITEM ( '' )  );
#8533 = CARTESIAN_POINT ( 'NONE',  ( -79.64356964374998427, -33.66562499938548569, 101.5914258081833879 ) ) ;
#8534 = CARTESIAN_POINT ( 'NONE',  ( -83.77821517812500929, -32.87812499938548427, -97.61286128772489690 ) ) ;
#8535 = CARTESIAN_POINT ( 'NONE',  ( 83.20384757729333103, -33.18615380933863435, -96.99999999999997158 ) ) ;
#8536 = CARTESIAN_POINT ( 'NONE',  ( 79.64356964374999848, -33.17812499938548854, -99.99999999999998579 ) ) ;
#8537 = CARTESIAN_POINT ( 'NONE',  ( 229.8435696437499303, -34.19062499938547717, -50.00000000000011369 ) ) ;
#8538 = CARTESIAN_POINT ( 'NONE',  ( -81.02178482187500208, -33.44062499938548427, 97.61286128772489690 ) ) ;
#8539 = CARTESIAN_POINT ( 'NONE',  ( 85.15643035625001289, -31.94062499938548427, -99.99999999999998579 ) ) ;
#8540 = ORIENTED_EDGE ( 'NONE', *, *, #12814, .T. ) ;
#8541 = CARTESIAN_POINT ( 'NONE',  ( 79.64356964375001269, -34.11562499938548854, 98.40857419181659793 ) ) ;
#8542 = CARTESIAN_POINT ( 'NONE',  ( 99.99999999999998579, 0.000000000000000000, 150.0000000000000000 ) ) ;
#8543 = CARTESIAN_POINT ( 'NONE',  ( -83.90000000000000568, -33.52499999999999858, 102.5980762113533018 ) ) ;
#8544 = CARTESIAN_POINT ( 'NONE',  ( -83.77821517812500929, -34.26562499938548711, 97.61286128772489690 ) ) ;
#8545 = CARTESIAN_POINT ( 'NONE',  ( -85.15643035624999868, -30.17812499938548498, 98.40857419181659793 ) ) ;
#8546 = ORIENTED_EDGE ( 'NONE', *, *, #5469, .T. ) ;
#8547 = DIRECTION ( 'NONE',  ( 0.000000000000000000, 0.000000000000000000, 1.000000000000000000 ) ) ;
#8548 = CARTESIAN_POINT ( 'NONE',  ( 233.9782151781249411, -32.99062499938548143, 97.61286128772489690 ) ) ;
#8549 = CARTESIAN_POINT ( 'NONE',  ( 99.99999999999997158, -5.200000000000008171, -100.0000000000000000 ) ) ;
#8550 = CARTESIAN_POINT ( 'NONE',  ( 83.90000000000000568, -33.67500000000000426, -97.40192378864668399 ) ) ;
#8551 = CARTESIAN_POINT ( 'NONE',  ( 3.974175853610046438, 3.450041667725685102, -1.156004144283996116 ) ) ;
#8552 = ADVANCED_FACE ( 'NONE', ( #12226 ), #3531, .F. ) ;
#8553 = CARTESIAN_POINT ( 'NONE',  ( 105.1999999999999744, -29.80000000000002203, 150.0000000000000000 ) ) ;
#8554 = CARTESIAN_POINT ( 'NONE',  ( 84.56803305035323604, -32.00000000000000000, 98.28830862702034210 ) ) ;
#8555 = CARTESIAN_POINT ( 'NONE',  ( 85.15643035624999868, -30.66562499938548569, 98.40857419181659793 ) ) ;
#8556 = CARTESIAN_POINT ( 'NONE',  ( 234.1999394931800396, -32.00000000000002132, 97.54622936382085641 ) ) ;
#8557 = LINE ( 'NONE', #9839, #18697 ) ;
#8558 = CARTESIAN_POINT ( 'NONE',  ( 82.39999999999999147, -34.64062499938548711, -103.1828516163667899 ) ) ;
#8559 = CARTESIAN_POINT ( 'NONE',  ( 80.90000000000000568, -32.94374999877096855, 97.40192378864668399 ) ) ;
#8560 =( BOUNDED_CURVE ( )  B_SPLINE_CURVE ( 2, ( #119, #19258, #6068, #4598, #12114, #9176, #9078, #7714, #10555 ),
 .UNSPECIFIED., .F., .F. ) 
 B_SPLINE_CURVE_WITH_KNOTS ( ( 3, 2, 2, 2, 3 ),
 ( 0.4374999999999999445, 0.4444444444444444198, 0.4583333333333333148, 0.4722222222222222099, 0.4791666666666665186 ),
 .UNSPECIFIED. ) 
 CURVE ( )  GEOMETRIC_REPRESENTATION_ITEM ( )  RATIONAL_B_SPLINE_CURVE ( ( 0.9330127018922192983, 0.9330127018922187432, 1.000000000000000000, 0.8660254037844387076, 1.000000000000000000, 0.8660254037844387076, 1.000000000000000000, 0.9330127018922207416, 0.9330127018922194093 ) ) 
 REPRESENTATION_ITEM ( '' )  );
#8561 = EDGE_LOOP ( 'NONE', ( #13306, #8906, #2932, #15688 ) ) ;
#8562 = CARTESIAN_POINT ( 'NONE',  ( 79.39999999999999147, -32.38124999877096855, 101.7320508075688821 ) ) ;
#8563 = ITEM_DEFINED_TRANSFORMATION ( 'NONE', 'NONE', #17679,  #10540 ) ;
#8564 = CARTESIAN_POINT ( 'NONE',  ( 233.9782151781249411, -35.05312499938548143, 102.3871387122750889 ) ) ;
#8565 = CARTESIAN_POINT ( 'NONE',  ( 233.9782151781249411, -34.00312499938547717, -52.38713871227520968 ) ) ;
#8566 = DIRECTION ( 'NONE',  ( -0.000000000000000000, -1.000000000000000000, -0.000000000000000000 ) ) ;
#8567 = CARTESIAN_POINT ( 'NONE',  ( 232.5999999999999659, -32.58749999999999858, -47.00000000000011369 ) ) ;
#8568 = VERTEX_POINT ( 'NONE', #4817 ) ;
#8569 = CARTESIAN_POINT ( 'NONE',  ( -85.15643035625001289, -33.74062499938548854, -99.99999999999998579 ) ) ;
#8570 = CARTESIAN_POINT ( 'NONE',  ( 111.0000000000000142, 15.19999999999997797, -150.0000000000000000 ) ) ;
#8571 = EDGE_LOOP ( 'NONE', ( #2928, #16701, #1345, #1754 ) ) ;
#8572 = APPLICATION_CONTEXT ( 'automotive_design' ) ;
#8573 = CARTESIAN_POINT ( 'NONE',  ( -82.40000000000000568, -32.08124999877097139, 102.9999999999999858 ) ) ;
#8574 = CARTESIAN_POINT ( 'NONE',  ( -79.64356964375001269, -30.51562499938548711, -98.40857419181659793 ) ) ;
#8575 = PLANE ( 'NONE',  #5507 ) ;
#8576 = CARTESIAN_POINT ( 'NONE',  ( 82.40000000000000568, -34.55624999877097281, -97.00000000000000000 ) ) ;
#8577 = CARTESIAN_POINT ( 'NONE',  ( -85.40000000000000568, -30.37603797259972893, 100.9999487804559664 ) ) ;
#8578 = CARTESIAN_POINT ( 'NONE',  ( -83.77821517812500929, -32.12812499938548427, 97.61286128772489690 ) ) ;
#8579 = CARTESIAN_POINT ( 'NONE',  ( 0.000000000000000000, -29.80000000000002203, 153.0000000000000000 ) ) ;
#8580 = VECTOR ( 'NONE', #17890, 1000.000000000000000 ) ;
#8581 = PRODUCT_DEFINITION_SHAPE ( 'NONE', 'NONE',  #14778 ) ;
#8582 = CARTESIAN_POINT ( 'NONE',  ( 82.39999999999999147, -30.73124999877096641, -103.4641016151377499 ) ) ;
#8583 = CARTESIAN_POINT ( 'NONE',  ( 231.0999999999999375, -30.97499999999999432, 97.40192378864668399 ) ) ;
#8584 = VERTEX_POINT ( 'NONE', #10855 ) ;
#8585 = DIRECTION ( 'NONE',  ( 0.000000000000000000, 0.000000000000000000, 1.000000000000000000 ) ) ;
#8586 =( NAMED_UNIT ( * ) SI_UNIT ( $, .STERADIAN. ) SOLID_ANGLE_UNIT ( ) );
#8587 = CARTESIAN_POINT ( 'NONE',  ( 231.0999999999999375, -32.71874999877096002, 97.40192378864668399 ) ) ;
#8588 = CARTESIAN_POINT ( 'NONE',  ( 229.5999999999999375, -30.88124999877096144, -51.73205080756898866 ) ) ;
#8589 = CARTESIAN_POINT ( 'NONE',  ( 232.5999999999999375, -29.99999999999999645, -53.00000000000012079 ) ) ;
#8590 = EDGE_CURVE ( 'NONE', #14649, #12940, #14130, .T. ) ;
#8591 = CARTESIAN_POINT ( 'NONE',  ( -85.15643035625001289, -31.00312499938548427, 101.5914258081833879 ) ) ;
#8592 = ORIENTED_EDGE ( 'NONE', *, *, #3514, .F. ) ;
#8593 = ORIENTED_EDGE ( 'NONE', *, *, #7013, .T. ) ;
#8594 = CARTESIAN_POINT ( 'NONE',  ( -80.90000000000000568, -34.20000000000000284, -102.5980762113533018 ) ) ;
#8595 = VECTOR ( 'NONE', #13135, 1000.000000000000227 ) ;
#8596 = CARTESIAN_POINT ( 'NONE',  ( 4.050536630291688311, 2.401306687817038821, -2.976670123173768001 ) ) ;
#8597 = ORIENTED_EDGE ( 'NONE', *, *, #15566, .T. ) ;
#8598 = DIRECTION ( 'NONE',  ( 1.000000000000000000, 0.000000000000000000, 0.000000000000000000 ) ) ;
#8599 = CARTESIAN_POINT ( 'NONE',  ( 82.39999999999999147, -33.03750000000000142, -103.4641016151377499 ) ) ;
#8600 = CARTESIAN_POINT ( 'NONE',  ( -4.000000000000000000, -7.806255641895631925E-15, -3.142992957459232350 ) ) ;
#8601 =( BOUNDED_CURVE ( )  B_SPLINE_CURVE ( 2, ( #6925, #2421, #13154, #19125, #1153, #2807, #5743, #9850, #4273 ),
 .UNSPECIFIED., .F., .F. ) 
 B_SPLINE_CURVE_WITH_KNOTS ( ( 3, 2, 2, 2, 3 ),
 ( 0.6874999999999997780, 0.6944444444444444198, 0.7083333333333333703, 0.7222222222222222099, 0.7291666666666665186 ),
 .UNSPECIFIED. ) 
 CURVE ( )  GEOMETRIC_REPRESENTATION_ITEM ( )  RATIONAL_B_SPLINE_CURVE ( ( 0.9330127018922194093, 0.9330127018922171889, 1.000000000000000000, 0.8660254037844387076, 1.000000000000000000, 0.8660254037844387076, 1.000000000000000000, 0.9330127018922209636, 0.9330127018922194093 ) ) 
 REPRESENTATION_ITEM ( '' )  );
#8602 = CARTESIAN_POINT ( 'NONE',  ( -85.15643035625001289, -30.70312499938548711, 99.99999999999998579 ) ) ;
#8603 = CARTESIAN_POINT ( 'NONE',  ( -85.40000000000000568, -31.31250000000000000, 101.7320508075688679 ) ) ;
#8604 = CYLINDRICAL_SURFACE ( 'NONE', #13980, 3.000000000000002665 ) ;
#8605 = DIRECTION ( 'NONE',  ( 1.000000000000000000, 0.000000000000000000, -0.000000000000000000 ) ) ;
#8606 = CARTESIAN_POINT ( 'NONE',  ( 82.65333140691207348, -34.99995246259152992, 102.9892844631211943 ) ) ;
#8607 = CARTESIAN_POINT ( 'NONE',  ( -82.40000000000000568, -30.00000000000000355, 103.0000000000000000 ) ) ;
#8608 = AXIS2_PLACEMENT_3D ( 'NONE', #15749, #10862, #5016 ) ;
#8609 = CARTESIAN_POINT ( 'NONE',  ( 229.8435696437499871, -31.00312499938547361, 101.5914258081833879 ) ) ;
#8610 = VERTEX_POINT ( 'NONE', #11047 ) ;
#8611 = SURFACE_STYLE_USAGE ( .BOTH. , #10281 ) ;
#8612 = CARTESIAN_POINT ( 'NONE',  ( -82.39999999999999147, -31.37812499938548427, -96.81714838363319586 ) ) ;
#8613 = CARTESIAN_POINT ( 'NONE',  ( 233.5140320577117166, -34.99999999999999289, 97.18639806692216609 ) ) ;
#8614 = CARTESIAN_POINT ( 'NONE',  ( -1.257172072275743346, 3.892973519171203378, -3.433252694550776862 ) ) ;
#8615 = CARTESIAN_POINT ( 'NONE',  ( 235.3564303562499731, -34.98839802032724577, 100.4359666841262708 ) ) ;
#8616 = CARTESIAN_POINT ( 'NONE',  ( -82.39999999999999147, -31.37812499938548427, 103.1828516163667899 ) ) ;
#8617 = CARTESIAN_POINT ( 'NONE',  ( -82.40000000000000568, -33.93750000000000711, 102.9999999999999858 ) ) ;
#8618 = CARTESIAN_POINT ( 'NONE',  ( 235.3564303562499447, -31.67812499938547788, -51.59142580818350865 ) ) ;
#8619 = ORIENTED_EDGE ( 'NONE', *, *, #13546, .T. ) ;
#8620 = CARTESIAN_POINT ( 'NONE',  ( -79.64356964374999848, -33.51562499938548711, 99.99999999999998579 ) ) ;
#8621 = FACE_OUTER_BOUND ( 'NONE', #4083, .T. ) ;
#8622 = CARTESIAN_POINT ( 'NONE',  ( 85.15643035624999868, -35.05312499938548143, 98.40857419181659793 ) ) ;
#8623 = CARTESIAN_POINT ( 'NONE',  ( -83.90000000000000568, -32.77499999999999858, 97.40192378864668399 ) ) ;
#8624 = CARTESIAN_POINT ( 'NONE',  ( 233.9782151781249411, -32.09062499938547575, 97.61286128772489690 ) ) ;
#8625 = CARTESIAN_POINT ( 'NONE',  ( 233.9782151781249411, -32.54062499938547859, -52.38713871227520968 ) ) ;
#8626 = LINE ( 'NONE', #10198, #10206 ) ;
#8627 = CARTESIAN_POINT ( 'NONE',  ( -82.39999999999999147, -33.96562499938548285, -103.1828516163667899 ) ) ;
#8628 = CARTESIAN_POINT ( 'NONE',  ( 81.02178482187500208, -34.79062499938548569, 102.3871387122750889 ) ) ;
#8629 = CARTESIAN_POINT ( 'NONE',  ( 81.02178482187500208, -35.05312499938548854, -102.3871387122750889 ) ) ;
#8630 = CARTESIAN_POINT ( 'NONE',  ( 235.5999999999999943, -30.18749999999999289, -51.73205080756900287 ) ) ;
#8631 = CARTESIAN_POINT ( 'NONE',  ( -82.39999999999999147, -33.17812499938548854, 103.1828516163667899 ) ) ;
#8632 = CARTESIAN_POINT ( 'NONE',  ( 81.02178482187500208, -31.79062499938548925, -102.3871387122750889 ) ) ;
#8633 = EDGE_CURVE ( 'NONE', #13113, #13520, #9446, .T. ) ;
#8634 = ORIENTED_EDGE ( 'NONE', *, *, #11640, .F. ) ;
#8635 = CARTESIAN_POINT ( 'NONE',  ( 85.15643035625001289, -34.75312499938548427, 99.99999999999998579 ) ) ;
#8636 = FACE_OUTER_BOUND ( 'NONE', #11551, .T. ) ;
#8637 = CARTESIAN_POINT ( 'NONE',  ( -82.39999999999999147, -33.48750000000000426, 103.4641016151377499 ) ) ;
#8638 = CARTESIAN_POINT ( 'NONE',  ( -79.64356964375001269, -32.57812499938548001, 98.40857419181659793 ) ) ;
#8639 = ORIENTED_EDGE ( 'NONE', *, *, #15450, .F. ) ;
#8640 = DIRECTION ( 'NONE',  ( -0.000000000000000000, -0.000000000000000000, -1.000000000000000000 ) ) ;
#8641 = VECTOR ( 'NONE', #6370, 1000.000000000000000 ) ;
#8642 = CARTESIAN_POINT ( 'NONE',  ( 232.5999999999999943, -33.62812499938547717, 103.1828516163667899 ) ) ;
#8643 = CARTESIAN_POINT ( 'NONE',  ( 79.69416654173913628, -34.99999999999998579, -100.6274906301335648 ) ) ;
#8644 = CARTESIAN_POINT ( 'NONE',  ( -82.40000000000001990, -32.13750000000000284, 103.0000000000000000 ) ) ;
#8645 = AXIS2_PLACEMENT_3D ( 'NONE', #4762, #8853, #1435 ) ;
#8646 = EDGE_CURVE ( 'NONE', #12516, #7903, #1950, .T. ) ;
#8647 = CARTESIAN_POINT ( 'NONE',  ( 113.0000000000000142, 15.19999999999994955, 50.00000000000001421 ) ) ;
#8648 = CARTESIAN_POINT ( 'NONE',  ( 82.40000000000000568, -30.00000000000000355, -99.99999999999998579 ) ) ;
#8649 = CARTESIAN_POINT ( 'NONE',  ( -85.40000000000000568, -32.68124999877097281, 98.26794919243111792 ) ) ;
#8650 = CARTESIAN_POINT ( 'NONE',  ( 85.15643035624999868, -31.64062499938548356, 101.5914258081833879 ) ) ;
#8651 = EDGE_CURVE ( 'NONE', #12903, #11485, #13809, .T. ) ;
#8652 = CARTESIAN_POINT ( 'NONE',  ( 232.8516854624778318, -32.00000000000002132, 97.14155664245926403 ) ) ;
#8653 = AXIS2_PLACEMENT_3D ( 'NONE', #8713, #1302, #11555 ) ;
#8654 = CARTESIAN_POINT ( 'NONE',  ( 111.0000000000000000, 10.19999999999997620, -139.9999999999999716 ) ) ;
#8655 = CARTESIAN_POINT ( 'NONE',  ( 79.64356964375001269, -33.59062499938548285, -98.40857419181659793 ) ) ;
#8656 = FACE_OUTER_BOUND ( 'NONE', #9072, .T. ) ;
#8657 = VERTEX_POINT ( 'NONE', #14264 ) ;
#8658 = CARTESIAN_POINT ( 'NONE',  ( 83.90000000000000568, -33.01874999877097139, 97.40192378864668399 ) ) ;
#8659 = ITEM_DEFINED_TRANSFORMATION ( 'NONE', 'NONE', #2373,  #10540 ) ;
#8660 = CARTESIAN_POINT ( 'NONE',  ( 229.8435696437499303, -35.20312499938548001, 99.99999999999998579 ) ) ;
#8661 = CARTESIAN_POINT ( 'NONE',  ( 229.8435696437499303, -35.20312499938548001, -50.00000000000011369 ) ) ;
#8662 = AXIS2_PLACEMENT_3D ( 'NONE', #7652, #19200, #4347 ) ;
#8663 = AXIS2_PLACEMENT_3D ( 'NONE', #6428, #12187, #16780 ) ;
#8664 = CARTESIAN_POINT ( 'NONE',  ( -85.15643035624999868, -34.67812499938548143, 98.40857419181659793 ) ) ;
#8665 = PLANE ( 'NONE',  #16476 ) ;
#8666 = EDGE_LOOP ( 'NONE', ( #1606, #14813, #5814, #6254, #18545 ) ) ;
#8667 = EDGE_CURVE ( 'NONE', #12107, #14117, #14433, .T. ) ;
#8668 = CARTESIAN_POINT ( 'NONE',  ( -85.15643035624999868, -35.11426541925033007, -101.0032526477118751 ) ) ;
#8669 = DIRECTION ( 'NONE',  ( -0.000000000000000000, 0.000000000000000000, -1.000000000000000000 ) ) ;
#8670 = ORIENTED_EDGE ( 'NONE', *, *, #13546, .F. ) ;
#8671 = CARTESIAN_POINT ( 'NONE',  ( -83.90000000000000568, -32.11874999877097281, 102.5980762113533018 ) ) ;
#8672 = CONICAL_SURFACE ( 'NONE', #266, 2.059999999999998721, 0.9599310885968738161 ) ;
#8673 = CARTESIAN_POINT ( 'NONE',  ( -79.64356964374999848, -30.92812499938548498, -99.99999999999998579 ) ) ;
#8674 = CARTESIAN_POINT ( 'NONE',  ( 231.7961524227065695, -34.40759618943233988, -47.00000000000011369 ) ) ;
#8675 = CARTESIAN_POINT ( 'NONE',  ( -82.39999999999999147, -32.30624999877097281, -103.4641016151377499 ) ) ;
#8676 = CARTESIAN_POINT ( 'NONE',  ( 229.8435696437499871, -31.19062499938548072, 98.40857419181659793 ) ) ;
#8677 = CARTESIAN_POINT ( 'NONE',  ( -85.40000000000000568, -33.95624999877097139, 101.7320508075688679 ) ) ;
#8678 = CARTESIAN_POINT ( 'NONE',  ( -85.15643035625001289, -31.60312499938548569, 99.99999999999998579 ) ) ;
#8679 = VECTOR ( 'NONE', #12572, 1000.000000000000000 ) ;
#8680 = CARTESIAN_POINT ( 'NONE',  ( -79.64356964374999848, -33.06562499938548427, -99.99999999999998579 ) ) ;
#8681 = DIRECTION ( 'NONE',  ( 0.000000000000000000, 0.000000000000000000, 1.000000000000000000 ) ) ;
#8682 = AXIS2_PLACEMENT_3D ( 'NONE', #4865, #3286, #5332 ) ;
#8683 =( BOUNDED_SURFACE ( )  B_SPLINE_SURFACE ( 1, 2, ( 
 ( #12062, #10884, #2976, #10500, #14895, #8932, #16466, #7857, #7569, #10786, #9218, #7659, #15181, #17933, #1799, #12260, #13718, #6112, #7765, #258, #18037, #4650, #10599, #4843, #1525, #6214, #359, #16748, #16564, #3362, #15089, #15581, #5331, #6594, #18415, #5429, #3558, #12540, #644, #15381, #543, #11268, #2192, #10975, #18612, #3457, #931, #5227, #835, #11074, #6693, #12837, #14197, #8149, #8339, #7953, #9808, #14296, #9515, #6887, #13906, #12636, #18803, #17236, #17141, #11175, #16946, #15481, #16853, #9414, #6795, #12742, #15770, #3746, #1996, #17043, #6499, #12447, #18513, #5035, #18710, #2092, #9712, #3654, #3842, #8050, #14006, #15674, #5130, #2283, #9620, #14100, #738, #8246, #2379, #13117, #7068, #4236, #4334, #11367, #16057, #8723, #17434, #14386, #1108, #14478, #17723, #18899, #10101, #6977, #11753, #5708, #8433, #2565, #5520, #10193, #13313, #1025, #7356, #14676, #2661, #4045, #8528, #10294, #16155, #10004, #12928, #19088, #11467, #19287, #1311, #8622, #15959, #13025, #16254, #2767, #18996 ),
 ( #13214, #5618, #14776, #17333, #7259, #11563, #14573, #19185, #17526, #8820, #5801, #2863, #4138, #1404, #1210, #7167, #3942, #11657, #9908, #15871, #2477, #17621, #16637, #3241, #1689, #7641, #9105, #15068, #4521, #2148, #7454, #2957, #13504, #16546, #17915, #12237, #3053, #12040, #9199, #9016, #143, #3145, #14873, #13595, #15162, #6192, #6093, #13412, #3338, #13700, #12142, #14976, #11944, #16444, #10479, #1599, #14058, #4725, #7546, #18014, #341, #4627, #1780, #42, #6288, #16729, #11848, #5993, #10581, #236, #18111, #10668, #7743, #18205, #16347, #4824, #15531, #10764, #9298, #8105, #8912, #5902, #17816, #4426, #10385, #1502, #5475, #8476, #8201, #6933, #12592, #3892, #15630, #4089, #2519, #15914, #3995, #10051, #14434, #9669, #7024, #18757, #5376, #2330, #18661, #692, #8294, #9960, #17289, #17091, #9762, #11421, #11225, #9860, #17190, #1067, #15724, #6646, #12788, #17381, #5280, #12978, #14152, #3703, #18948, #3794, #5572, #14244, #16010, #18560, #18855, #882, #11324, #11519, #786, #17480, #2614 ) ),
 .UNSPECIFIED., .F., .F., .F. ) 
 B_SPLINE_SURFACE_WITH_KNOTS ( ( 2, 2 ),
 ( 3, 2, 2, 2, 2, 2, 2, 2, 2, 2, 2, 2, 2, 2, 2, 2, 2, 2, 2, 2, 2, 2, 2, 2, 2, 2, 2, 2, 2, 2, 2, 2, 2, 2, 2, 2, 2, 2, 2, 2, 2, 2, 2, 2, 2, 2, 2, 2, 2, 2, 2, 2, 2, 2, 2, 2, 2, 2, 2, 2, 2, 2, 2, 2, 2, 2, 2, 2, 3 ),
 ( 0.000000000000000000, 1.000000000000000000 ),
 ( 0.000000000000000000, 0.01388888888888888812, 0.02777777777777777624, 0.04166666666666666435, 0.05555555555555555247, 0.06944444444444444753, 0.08333333333333332871, 0.09722222222222222376, 0.1111111111111111049, 0.1250000000000000000, 0.1388888888888888951, 0.1527777777777777901, 0.1666666666666666574, 0.1805555555555555525, 0.1944444444444444475, 0.2083333333333333426, 0.2222222222222222099, 0.2361111111111111049, 0.2500000000000000000, 0.2638888888888888951, 0.2777777777777777901, 0.2916666666666666852, 0.3055555555555555802, 0.3194444444444444198, 0.3333333333333333148, 0.3472222222222222099, 0.3611111111111111049, 0.3750000000000000000, 0.3888888888888888951, 0.4027777777777777901, 0.4166666666666666852, 0.4305555555555555802, 0.4444444444444444198, 0.4583333333333333148, 0.4722222222222222099, 0.4861111111111111049, 0.5000000000000000000, 0.5138888888888888395, 0.5277777777777777901, 0.5416666666666666297, 0.5555555555555555802, 0.5694444444444444198, 0.5833333333333333703, 0.5972222222222222099, 0.6111111111111111605, 0.6250000000000000000, 0.6388888888888888395, 0.6527777777777777901, 0.6666666666666666297, 0.6805555555555555802, 0.6944444444444444198, 0.7083333333333333703, 0.7222222222222222099, 0.7361111111111111605, 0.7500000000000000000, 0.7638888888888888395, 0.7777777777777777901, 0.7916666666666666297, 0.8055555555555555802, 0.8194444444444444198, 0.8333333333333333703, 0.8472222222222222099, 0.8611111111111111605, 0.8750000000000000000, 0.8888888888888888395, 0.9027777777777777901, 0.9166666666666666297, 0.9258785066912882389, 0.9351372917582011501 ),
 .UNSPECIFIED. ) 
 GEOMETRIC_REPRESENTATION_ITEM ( )  RATIONAL_B_SPLINE_SURFACE ( (
 ( 1.000000000000000000, 0.8660254037844387076, 1.000000000000000000, 0.8660254037844387076, 1.000000000000000000, 0.8660254037844387076, 1.000000000000000000, 0.8660254037844387076, 1.000000000000000000, 0.8660254037844387076, 1.000000000000000000, 0.8660254037844387076, 1.000000000000000000, 0.8660254037844387076, 1.000000000000000000, 0.8660254037844387076, 1.000000000000000000, 0.8660254037844387076, 1.000000000000000000, 0.8660254037844387076, 1.000000000000000000, 0.8660254037844387076, 1.000000000000000000, 0.8660254037844387076, 1.000000000000000000, 0.8660254037844387076, 1.000000000000000000, 0.8660254037844387076, 1.000000000000000000, 0.8660254037844387076, 1.000000000000000000, 0.8660254037844387076, 1.000000000000000000, 0.8660254037844387076, 1.000000000000000000, 0.8660254037844387076, 1.000000000000000000, 0.8660254037844387076, 1.000000000000000000, 0.8660254037844387076, 1.000000000000000000, 0.8660254037844387076, 1.000000000000000000, 0.8660254037844387076, 1.000000000000000000, 0.8660254037844387076, 1.000000000000000000, 0.8660254037844387076, 1.000000000000000000, 0.8660254037844387076, 1.000000000000000000, 0.8660254037844387076, 1.000000000000000000, 0.8660254037844387076, 1.000000000000000000, 0.8660254037844387076, 1.000000000000000000, 0.8660254037844387076, 1.000000000000000000, 0.8660254037844387076, 1.000000000000000000, 0.8660254037844387076, 1.000000000000000000, 0.8660254037844387076, 1.000000000000000000, 0.8660254037844387076, 1.000000000000000000, 0.8660254037844387076, 1.000000000000000000, 0.8660254037844387076, 1.000000000000000000, 0.8660254037844387076, 1.000000000000000000, 0.8660254037844387076, 1.000000000000000000, 0.8660254037844387076, 1.000000000000000000, 0.8660254037844387076, 1.000000000000000000, 0.8660254037844387076, 1.000000000000000000, 0.8660254037844387076, 1.000000000000000000, 0.8660254037844387076, 1.000000000000000000, 0.8660254037844387076, 1.000000000000000000, 0.8660254037844387076, 1.000000000000000000, 0.8660254037844387076, 1.000000000000000000, 0.8660254037844387076, 1.000000000000000000, 0.8660254037844387076, 1.000000000000000000, 0.8660254037844387076, 1.000000000000000000, 0.8660254037844387076, 1.000000000000000000, 0.8660254037844387076, 1.000000000000000000, 0.8660254037844387076, 1.000000000000000000, 0.8660254037844387076, 1.000000000000000000, 0.8660254037844387076, 1.000000000000000000, 0.8660254037844387076, 1.000000000000000000, 0.8660254037844387076, 1.000000000000000000, 0.8660254037844387076, 1.000000000000000000, 0.8660254037844387076, 1.000000000000000000, 0.8660254037844387076, 1.000000000000000000, 0.8660254037844387076, 1.000000000000000000, 0.8660254037844387076, 1.000000000000000000, 0.8660254037844387076, 1.000000000000000000, 0.8660254037844387076, 1.000000000000000000, 0.8660254037844387076, 1.000000000000000000, 0.8660254037844387076, 1.000000000000000000, 0.8660254037844387076, 1.000000000000000000, 0.8660254037844387076, 1.000000000000000000, 0.9111410165655264848, 0.9401539157124900736, 0.9401539157124900736, 0.9401539157124900736),
 ( 1.000000000000000000, 0.8660254037844387076, 1.000000000000000000, 0.8660254037844387076, 1.000000000000000000, 0.8660254037844387076, 1.000000000000000000, 0.8660254037844387076, 1.000000000000000000, 0.8660254037844387076, 1.000000000000000000, 0.8660254037844387076, 1.000000000000000000, 0.8660254037844387076, 1.000000000000000000, 0.8660254037844387076, 1.000000000000000000, 0.8660254037844387076, 1.000000000000000000, 0.8660254037844387076, 1.000000000000000000, 0.8660254037844387076, 1.000000000000000000, 0.8660254037844387076, 1.000000000000000000, 0.8660254037844387076, 1.000000000000000000, 0.8660254037844387076, 1.000000000000000000, 0.8660254037844387076, 1.000000000000000000, 0.8660254037844387076, 1.000000000000000000, 0.8660254037844387076, 1.000000000000000000, 0.8660254037844387076, 1.000000000000000000, 0.8660254037844387076, 1.000000000000000000, 0.8660254037844387076, 1.000000000000000000, 0.8660254037844387076, 1.000000000000000000, 0.8660254037844387076, 1.000000000000000000, 0.8660254037844387076, 1.000000000000000000, 0.8660254037844387076, 1.000000000000000000, 0.8660254037844387076, 1.000000000000000000, 0.8660254037844387076, 1.000000000000000000, 0.8660254037844387076, 1.000000000000000000, 0.8660254037844387076, 1.000000000000000000, 0.8660254037844387076, 1.000000000000000000, 0.8660254037844387076, 1.000000000000000000, 0.8660254037844387076, 1.000000000000000000, 0.8660254037844387076, 1.000000000000000000, 0.8660254037844387076, 1.000000000000000000, 0.8660254037844387076, 1.000000000000000000, 0.8660254037844387076, 1.000000000000000000, 0.8660254037844387076, 1.000000000000000000, 0.8660254037844387076, 1.000000000000000000, 0.8660254037844387076, 1.000000000000000000, 0.8660254037844387076, 1.000000000000000000, 0.8660254037844387076, 1.000000000000000000, 0.8660254037844387076, 1.000000000000000000, 0.8660254037844387076, 1.000000000000000000, 0.8660254037844387076, 1.000000000000000000, 0.8660254037844387076, 1.000000000000000000, 0.8660254037844387076, 1.000000000000000000, 0.8660254037844387076, 1.000000000000000000, 0.8660254037844387076, 1.000000000000000000, 0.8660254037844387076, 1.000000000000000000, 0.8660254037844387076, 1.000000000000000000, 0.8660254037844387076, 1.000000000000000000, 0.8660254037844387076, 1.000000000000000000, 0.8660254037844387076, 1.000000000000000000, 0.8660254037844387076, 1.000000000000000000, 0.8660254037844387076, 1.000000000000000000, 0.8660254037844387076, 1.000000000000000000, 0.8660254037844387076, 1.000000000000000000, 0.8660254037844387076, 1.000000000000000000, 0.8660254037844387076, 1.000000000000000000, 0.8660254037844387076, 1.000000000000000000, 0.8660254037844387076, 1.000000000000000000, 0.8660254037844387076, 1.000000000000000000, 0.8660254037844387076, 1.000000000000000000, 0.8660254037844387076, 1.000000000000000000, 0.8660254037844387076, 1.000000000000000000, 0.8660254037844387076, 1.000000000000000000, 0.8660254037844387076, 1.000000000000000000, 0.9111410165655264848, 0.9401539157124900736, 0.9401539157124900736, 0.9401539157124900736) ) ) 
 REPRESENTATION_ITEM ( '' )  SURFACE ( )  );
#8684 = CARTESIAN_POINT ( 'NONE',  ( 232.5999999999999659, -32.13749999999999574, -47.00000000000011369 ) ) ;
#8685 = EDGE_CURVE ( 'NONE', #2327, #16779, #5257, .T. ) ;
#8686 = CARTESIAN_POINT ( 'NONE',  ( 79.39999999999999147, -30.61874999877096926, -99.99999999999998579 ) ) ;
#8687 = CARTESIAN_POINT ( 'NONE',  ( 234.0999999999999375, -30.59999999999999432, 97.40192378864668399 ) ) ;
#8688 = EDGE_LOOP ( 'NONE', ( #172, #8018, #16737, #4840 ) ) ;
#8689 = DIRECTION ( 'NONE',  ( 0.000000000000000000, -3.336006684570784876E-15, -1.000000000000000000 ) ) ;
#8690 = PRESENTATION_STYLE_ASSIGNMENT (( #16120 ) ) ;
#8691 = CARTESIAN_POINT ( 'NONE',  ( 229.5999999999999375, -31.78124999877096357, 98.26794919243111792 ) ) ;
#8692 = CARTESIAN_POINT ( 'NONE',  ( 232.5999999999999375, -32.75624999877096144, -53.46410161513786363 ) ) ;
#8693 = CARTESIAN_POINT ( 'NONE',  ( -85.15643035625001289, -30.14062499938548711, 99.99999999999998579 ) ) ;
#8694 = VERTEX_POINT ( 'NONE', #8122 ) ;
#8695 = ORIENTED_EDGE ( 'NONE', *, *, #13166, .T. ) ;
#8696 = LINE ( 'NONE', #5683, #6028 ) ;
#8697 = CIRCLE ( 'NONE', #18650, 3.500000000000000000 ) ;
#8698 = CARTESIAN_POINT ( 'NONE',  ( -79.90595866893276877, -34.99999999999997868, -98.81289630734772800 ) ) ;
#8699 = DIRECTION ( 'NONE',  ( 0.000000000000000000, 0.000000000000000000, -1.000000000000000000 ) ) ;
#8700 = ORIENTED_EDGE ( 'NONE', *, *, #3245, .T. ) ;
#8701 = CARTESIAN_POINT ( 'NONE',  ( -83.20384757729335945, -31.65134618820330559, 102.9999999999999858 ) ) ;
#8702 = CARTESIAN_POINT ( 'NONE',  ( 83.41996205656103314, -34.99999999999999289, 102.8282615748025535 ) ) ;
#8703 = CARTESIAN_POINT ( 'NONE',  ( 0.000000000000000000, 3.755786496842902015E-16, 3.500000000000000000 ) ) ;
#8704 = CARTESIAN_POINT ( 'NONE',  ( -79.64356964374999848, -30.92812499938548498, 99.99999999999998579 ) ) ;
#8705 = CARTESIAN_POINT ( 'NONE',  ( -83.90000000000000568, -31.27500000000000568, 102.5980762113533018 ) ) ;
#8706 = CARTESIAN_POINT ( 'NONE',  ( 232.5999999999999659, -32.53124999877096712, -47.00000000000011369 ) ) ;
#8707 = CARTESIAN_POINT ( 'NONE',  ( 79.91954014136220508, -34.99999999999999289, 101.4427624130899375 ) ) ;
#8708 = LINE ( 'NONE', #13011, #7734 ) ;
#8709 = ORIENTED_EDGE ( 'NONE', *, *, #2920, .T. ) ;
#8710 = CARTESIAN_POINT ( 'NONE',  ( -85.15643035624999868, -30.55312499938548854, -98.40857419181659793 ) ) ;
#8711 = CARTESIAN_POINT ( 'NONE',  ( 233.4038475772933339, -32.38259618943233420, -53.00000000000011369 ) ) ;
#8712 = CARTESIAN_POINT ( 'NONE',  ( -4.175648173966055587, 2.207990556236529844, -3.469390959564062626 ) ) ;
#8713 = CARTESIAN_POINT ( 'NONE',  ( 111.0000000000000000, 10.19999999999997620, -139.9999999999999716 ) ) ;
#8714 = CARTESIAN_POINT ( 'NONE',  ( -79.64356964375001269, -30.40312499938548285, 101.5914258081833879 ) ) ;
#8715 = CARTESIAN_POINT ( 'NONE',  ( -82.39999999999999147, -34.16250000000000142, 97.00000000000000000 ) ) ;
#8716 = CARTESIAN_POINT ( 'NONE',  ( 233.9782151781249411, -33.14062499938548001, -47.61286128772501769 ) ) ;
#8717 =( BOUNDED_CURVE ( )  B_SPLINE_CURVE ( 2, ( #7408, #9159, #9253, #11901, #13371, #17873, #16687, #18068, #100 ),
 .UNSPECIFIED., .F., .F. ) 
 B_SPLINE_CURVE_WITH_KNOTS ( ( 3, 2, 2, 2, 3 ),
 ( 0.5208333333333331483, 0.5277777777777777901, 0.5416666666666666297, 0.5555555555555555802, 0.5625000000000001110 ),
 .UNSPECIFIED. ) 
 CURVE ( )  GEOMETRIC_REPRESENTATION_ITEM ( )  RATIONAL_B_SPLINE_CURVE ( ( 0.9330127018922194093, 0.9330127018922177440, 1.000000000000000000, 0.8660254037844387076, 1.000000000000000000, 0.8660254037844387076, 1.000000000000000000, 0.9330127018922182991, 0.9330127018922194093 ) ) 
 REPRESENTATION_ITEM ( '' )  );
#8718 = ORIENTED_EDGE ( 'NONE', *, *, #13559, .F. ) ;
#8719 = VERTEX_POINT ( 'NONE', #995 ) ;
#8720 = CARTESIAN_POINT ( 'NONE',  ( -84.53225329756190831, -32.00000000000000711, 98.24409948398896120 ) ) ;
#8721 = CARTESIAN_POINT ( 'NONE',  ( -79.64356964375001269, -34.90312499938548285, 101.5914258081833879 ) ) ;
#8722 = CARTESIAN_POINT ( 'NONE',  ( -83.95700771753406855, -35.00000000000000711, -102.5724980549416898 ) ) ;
#8723 = CARTESIAN_POINT ( 'NONE',  ( 79.64356964375001269, -33.92812499938548854, 101.5914258081833879 ) ) ;
#8724 = CARTESIAN_POINT ( 'NONE',  ( 85.40000000000000568, -34.05000000000000426, -99.99999999999998579 ) ) ;
#8725 = CARTESIAN_POINT ( 'NONE',  ( 235.3564303562499447, -31.75312499938547717, 101.5914258081833879 ) ) ;
#8726 = CARTESIAN_POINT ( 'NONE',  ( 231.2217848218749339, -34.11562499938548143, -47.61286128772501769 ) ) ;
#8727 = CARTESIAN_POINT ( 'NONE',  ( -84.51155386534844638, -35.25364837475780888, 98.22820752270799005 ) ) ;
#8728 = CARTESIAN_POINT ( 'NONE',  ( 82.39999999999999147, -32.98124999877096286, -102.9999999999999858 ) ) ;
#8729 = CARTESIAN_POINT ( 'NONE',  ( 81.02178482187500208, -31.64062499938548356, -97.61286128772489690 ) ) ;
#8730 = CARTESIAN_POINT ( 'NONE',  ( 231.0999999999999375, -30.52499999999999503, -52.59807621135342970 ) ) ;
#8731 = CARTESIAN_POINT ( 'NONE',  ( -85.15643035625001289, -32.35312499938548569, 101.5914258081833879 ) ) ;
#8732 = CARTESIAN_POINT ( 'NONE',  ( 82.39999999999999147, -32.05312499938548854, -96.81714838363319586 ) ) ;
#8733 = ORIENTED_EDGE ( 'NONE', *, *, #12577, .T. ) ;
#8734 = CARTESIAN_POINT ( 'NONE',  ( 105.1999999999999602, -29.80000000000001492, -97.80000000000002558 ) ) ;
#8735 = CARTESIAN_POINT ( 'NONE',  ( 79.39999999999999147, -33.82500000000000284, -99.99999999999998579 ) ) ;
#8736 = CARTESIAN_POINT ( 'NONE',  ( 235.3564303562499447, -31.82812499938547646, -50.00000000000011369 ) ) ;
#8737 = CARTESIAN_POINT ( 'NONE',  ( -85.15643035624999868, -32.42812499938548854, 98.40857419181659793 ) ) ;
#8738 = VERTEX_POINT ( 'NONE', #902 ) ;
#8739 = CARTESIAN_POINT ( 'NONE',  ( -83.20395887649198130, -35.00000000000002132, 102.6365808225363025 ) ) ;
#8740 = EDGE_CURVE ( 'NONE', #1665, #6484, #3462, .T. ) ;
#8741 = DIRECTION ( 'NONE',  ( 0.000000000000000000, 0.000000000000000000, -1.000000000000000000 ) ) ;
#8742 = CARTESIAN_POINT ( 'NONE',  ( 79.64057174634724845, -34.99999999999999289, -100.3964642588221494 ) ) ;
#8743 = CARTESIAN_POINT ( 'NONE',  ( -85.40000000000000568, -32.28356250001229455, 98.26794919243111792 ) ) ;
#8744 = ADVANCED_FACE ( 'NONE', ( #11341 ), #12832, .F. ) ;
#8745 = EDGE_CURVE ( 'NONE', #14868, #14513, #4065, .T. ) ;
#8746 = CARTESIAN_POINT ( 'NONE',  ( -82.40000000000000568, -32.00000000000000000, -99.99999999999998579 ) ) ;
#8747 = CARTESIAN_POINT ( 'NONE',  ( 230.7036604445367232, -32.00000000000000711, -47.97042480180352442 ) ) ;
#8748 = CARTESIAN_POINT ( 'NONE',  ( -79.64356964375001269, -32.65312499938548285, 101.5914258081833879 ) ) ;
#8749 = CARTESIAN_POINT ( 'NONE',  ( -82.40000000000001990, -32.53124999877097423, 103.0000000000000000 ) ) ;
#8750 = CARTESIAN_POINT ( 'NONE',  ( 79.64356964375001269, -33.21562499938548996, 98.40857419181659793 ) ) ;
#8751 = CARTESIAN_POINT ( 'NONE',  ( 110.9999999999999574, -21.80000000000003268, -139.9999999999999716 ) ) ;
#8752 = DIRECTION ( 'NONE',  ( 0.000000000000000000, 0.000000000000000000, -1.000000000000000000 ) ) ;
#8753 = CARTESIAN_POINT ( 'NONE',  ( 79.64356964375001269, -33.14062499938548711, -98.40857419181659793 ) ) ;
#8754 = CARTESIAN_POINT ( 'NONE',  ( -79.64356964374999848, -31.82812499938548356, -99.99999999999998579 ) ) ;
#8755 = VERTEX_POINT ( 'NONE', #3021 ) ;
#8756 = CARTESIAN_POINT ( 'NONE',  ( 79.39999999999999147, -32.86874999877097281, 99.99999999999998579 ) ) ;
#8757 = ITEM_DEFINED_TRANSFORMATION ( 'NONE', 'NONE', #10492,  #10540 ) ;
#8758 = CARTESIAN_POINT ( 'NONE',  ( -0.3208286057739654917, 4.433571671609680465, -0.3503314178412548774 ) ) ;
#8759 = CARTESIAN_POINT ( 'NONE',  ( 230.4884461346514968, -35.25364837475780178, -51.77179247729210942 ) ) ;
#8760 = EDGE_CURVE ( 'NONE', #6188, #6906, #8696, .T. ) ;
#8761 = CARTESIAN_POINT ( 'NONE',  ( -83.77821517812500929, -30.32812499938548711, 97.61286128772489690 ) ) ;
#8762 = CARTESIAN_POINT ( 'NONE',  ( 83.52022063339155977, -31.99999999999999289, 102.5731757465994036 ) ) ;
#8763 = EDGE_LOOP ( 'NONE', ( #7752, #6284, #14948, #9162 ) ) ;
#8764 = EDGE_CURVE ( 'NONE', #7775, #14052, #7140, .T. ) ;
#8765 = CARTESIAN_POINT ( 'NONE',  ( -85.15643035625001289, -32.84062499938548285, -99.99999999999998579 ) ) ;
#8766 = EDGE_CURVE ( 'NONE', #3532, #13429, #8511, .T. ) ;
#8767 = CARTESIAN_POINT ( 'NONE',  ( 0.02944718078427176200, -0.6813962075686350595, -3.500000000000000000 ) ) ;
#8768 = ORIENTED_EDGE ( 'NONE', *, *, #10557, .F. ) ;
#8769 = CARTESIAN_POINT ( 'NONE',  ( -82.40000000000000568, -30.33749999999999858, 102.9999999999999858 ) ) ;
#8770 = CARTESIAN_POINT ( 'NONE',  ( -82.39999999999999147, -34.41562499938547859, -103.1828516163667899 ) ) ;
#8771 =( BOUNDED_SURFACE ( )  B_SPLINE_SURFACE ( 1, 2, ( 
 ( #11378, #8351, #1221, #6987, #13127, #14305, #17444, #19007, #17632, #13036, #12938, #4151, #4247, #16067, #19097, #11280, #2389, #3855, #941, #5627, #12846, #1034, #15972, #9818, #4055, #11573, #18815, #2485, #5439, #2673, #15780, #17344, #3954, #5718, #10014, #9919, #8443, #2578, #15881, #11668, #10205, #16168, #1120, #14396, #8632, #18910, #5529, #11477, #8539, #2779, #7080, #8732, #1610, #7365, #8830, #16555, #4734, #9117, #3155, #19298, #14986, #10680, #11761, #13515, #2873, #5912, #16649, #9208, #17737, #15173, #6205, #1790, #14787, #17924, #1413, #14884, #15079, #16357, #3064, #2967, #1698, #6102, #16455, #1514, #4343, #4533, #7650, #9026, #10590, #10305, #7755, #13605, #4641, #16262, #4437, #13710, #13322, #246, #6003, #10491, #12153, #11857, #5812, #18120, #3250, #17825, #10395, #8922, #7463, #13424, #53, #11954, #7558, #152, #12051, #18027, #2066, #3628, #11148, #10955, #18296, #6570, #15556, #5109, #717, #9690, #7836, #16832, #4915, #339, #4822, #2170, #6473, #18202, #9489, #12331, #8127 ),
 ( #9590, #8024, #10861, #13790, #16924, #5015, #1778, #14078, #622, #3439, #9390, #6671, #15356, #12518, #3335, #12614, #18587, #7740, #15261, #1973, #3536, #433, #18488, #5201, #17117, #3725, #13698, #6286, #12233, #6378, #10762, #16726, #9296, #1876, #7930, #15456, #11051, #17018, #13881, #520, #13984, #12427, #18395, #11248, #19066, #17503, #11541, #18971, #11633, #3918, #18876, #17595, #8316, #14268, #4113, #1188, #15748, #10076, #11444, #17212, #18688, #7044, #14550, #5595, #13001, #9786, #5498, #2258, #1086, #6956, #17407, #906, #16032, #2635, #4022, #9982, #15937, #2540, #6866, #9883, #12811, #8599, #8500, #12908, #18778, #7145, #5403, #2456, #13095, #11345, #15845, #5685, #810, #5304, #8411, #4207, #14454, #3817, #15652, #8227, #14174, #17311, #2353, #6768, #12714, #14364, #999, #9241, #12084, #19257, #4861, #1383, #1823, #11725, #10806, #1914, #16131, #4307, #4669, #281, #2838, #15205, #12280, #9338, #7877, #2740, #3386, #14651, #16233, #6419, #1286, #17693, #13828, #8792, #6232, #7783, #13737 ) ),
 .UNSPECIFIED., .F., .F., .F. ) 
 B_SPLINE_SURFACE_WITH_KNOTS ( ( 2, 2 ),
 ( 3, 2, 2, 2, 2, 2, 2, 2, 2, 2, 2, 2, 2, 2, 2, 2, 2, 2, 2, 2, 2, 2, 2, 2, 2, 2, 2, 2, 2, 2, 2, 2, 2, 2, 2, 2, 2, 2, 2, 2, 2, 2, 2, 2, 2, 2, 2, 2, 2, 2, 2, 2, 2, 2, 2, 2, 2, 2, 2, 2, 2, 2, 2, 2, 2, 2, 2, 2, 3 ),
 ( 0.000000000000000000, 1.000000000000000000 ),
 ( 0.000000000000000000, 0.01388888888888888812, 0.02777777777777777624, 0.04166666666666666435, 0.05555555555555555247, 0.06944444444444444753, 0.08333333333333332871, 0.09722222222222222376, 0.1111111111111111049, 0.1250000000000000000, 0.1388888888888888951, 0.1527777777777777901, 0.1666666666666666574, 0.1805555555555555525, 0.1944444444444444475, 0.2083333333333333426, 0.2222222222222222099, 0.2361111111111111049, 0.2500000000000000000, 0.2638888888888888951, 0.2777777777777777901, 0.2916666666666666852, 0.3055555555555555802, 0.3194444444444444198, 0.3333333333333333148, 0.3472222222222222099, 0.3611111111111111049, 0.3750000000000000000, 0.3888888888888888951, 0.4027777777777777901, 0.4166666666666666852, 0.4305555555555555802, 0.4444444444444444198, 0.4583333333333333148, 0.4722222222222222099, 0.4861111111111111049, 0.5000000000000000000, 0.5138888888888888395, 0.5277777777777777901, 0.5416666666666666297, 0.5555555555555555802, 0.5694444444444444198, 0.5833333333333333703, 0.5972222222222222099, 0.6111111111111111605, 0.6250000000000000000, 0.6388888888888888395, 0.6527777777777777901, 0.6666666666666666297, 0.6805555555555555802, 0.6944444444444444198, 0.7083333333333333703, 0.7222222222222222099, 0.7361111111111111605, 0.7500000000000000000, 0.7638888888888888395, 0.7777777777777777901, 0.7916666666666666297, 0.8055555555555555802, 0.8194444444444444198, 0.8333333333333333703, 0.8472222222222222099, 0.8611111111111111605, 0.8750000000000000000, 0.8888888888888888395, 0.9027777777777777901, 0.9166666666666666297, 0.9258785066912882389, 0.9351372917582011501 ),
 .UNSPECIFIED. ) 
 GEOMETRIC_REPRESENTATION_ITEM ( )  RATIONAL_B_SPLINE_SURFACE ( (
 ( 1.000000000000000000, 0.8660254037844387076, 1.000000000000000000, 0.8660254037844387076, 1.000000000000000000, 0.8660254037844387076, 1.000000000000000000, 0.8660254037844387076, 1.000000000000000000, 0.8660254037844387076, 1.000000000000000000, 0.8660254037844387076, 1.000000000000000000, 0.8660254037844387076, 1.000000000000000000, 0.8660254037844387076, 1.000000000000000000, 0.8660254037844387076, 1.000000000000000000, 0.8660254037844387076, 1.000000000000000000, 0.8660254037844387076, 1.000000000000000000, 0.8660254037844387076, 1.000000000000000000, 0.8660254037844387076, 1.000000000000000000, 0.8660254037844387076, 1.000000000000000000, 0.8660254037844387076, 1.000000000000000000, 0.8660254037844387076, 1.000000000000000000, 0.8660254037844387076, 1.000000000000000000, 0.8660254037844387076, 1.000000000000000000, 0.8660254037844387076, 1.000000000000000000, 0.8660254037844387076, 1.000000000000000000, 0.8660254037844387076, 1.000000000000000000, 0.8660254037844387076, 1.000000000000000000, 0.8660254037844387076, 1.000000000000000000, 0.8660254037844387076, 1.000000000000000000, 0.8660254037844387076, 1.000000000000000000, 0.8660254037844387076, 1.000000000000000000, 0.8660254037844387076, 1.000000000000000000, 0.8660254037844387076, 1.000000000000000000, 0.8660254037844387076, 1.000000000000000000, 0.8660254037844387076, 1.000000000000000000, 0.8660254037844387076, 1.000000000000000000, 0.8660254037844387076, 1.000000000000000000, 0.8660254037844387076, 1.000000000000000000, 0.8660254037844387076, 1.000000000000000000, 0.8660254037844387076, 1.000000000000000000, 0.8660254037844387076, 1.000000000000000000, 0.8660254037844387076, 1.000000000000000000, 0.8660254037844387076, 1.000000000000000000, 0.8660254037844387076, 1.000000000000000000, 0.8660254037844387076, 1.000000000000000000, 0.8660254037844387076, 1.000000000000000000, 0.8660254037844387076, 1.000000000000000000, 0.8660254037844387076, 1.000000000000000000, 0.8660254037844387076, 1.000000000000000000, 0.8660254037844387076, 1.000000000000000000, 0.8660254037844387076, 1.000000000000000000, 0.8660254037844387076, 1.000000000000000000, 0.8660254037844387076, 1.000000000000000000, 0.8660254037844387076, 1.000000000000000000, 0.8660254037844387076, 1.000000000000000000, 0.8660254037844387076, 1.000000000000000000, 0.8660254037844387076, 1.000000000000000000, 0.8660254037844387076, 1.000000000000000000, 0.8660254037844387076, 1.000000000000000000, 0.8660254037844387076, 1.000000000000000000, 0.8660254037844387076, 1.000000000000000000, 0.8660254037844387076, 1.000000000000000000, 0.8660254037844387076, 1.000000000000000000, 0.8660254037844387076, 1.000000000000000000, 0.8660254037844387076, 1.000000000000000000, 0.8660254037844387076, 1.000000000000000000, 0.8660254037844387076, 1.000000000000000000, 0.8660254037844387076, 1.000000000000000000, 0.8660254037844387076, 1.000000000000000000, 0.8660254037844387076, 1.000000000000000000, 0.8660254037844387076, 1.000000000000000000, 0.9111410165655264848, 0.9401539157124900736, 0.9401539157124900736, 0.9401539157124900736),
 ( 1.000000000000000000, 0.8660254037844387076, 1.000000000000000000, 0.8660254037844387076, 1.000000000000000000, 0.8660254037844387076, 1.000000000000000000, 0.8660254037844387076, 1.000000000000000000, 0.8660254037844387076, 1.000000000000000000, 0.8660254037844387076, 1.000000000000000000, 0.8660254037844387076, 1.000000000000000000, 0.8660254037844387076, 1.000000000000000000, 0.8660254037844387076, 1.000000000000000000, 0.8660254037844387076, 1.000000000000000000, 0.8660254037844387076, 1.000000000000000000, 0.8660254037844387076, 1.000000000000000000, 0.8660254037844387076, 1.000000000000000000, 0.8660254037844387076, 1.000000000000000000, 0.8660254037844387076, 1.000000000000000000, 0.8660254037844387076, 1.000000000000000000, 0.8660254037844387076, 1.000000000000000000, 0.8660254037844387076, 1.000000000000000000, 0.8660254037844387076, 1.000000000000000000, 0.8660254037844387076, 1.000000000000000000, 0.8660254037844387076, 1.000000000000000000, 0.8660254037844387076, 1.000000000000000000, 0.8660254037844387076, 1.000000000000000000, 0.8660254037844387076, 1.000000000000000000, 0.8660254037844387076, 1.000000000000000000, 0.8660254037844387076, 1.000000000000000000, 0.8660254037844387076, 1.000000000000000000, 0.8660254037844387076, 1.000000000000000000, 0.8660254037844387076, 1.000000000000000000, 0.8660254037844387076, 1.000000000000000000, 0.8660254037844387076, 1.000000000000000000, 0.8660254037844387076, 1.000000000000000000, 0.8660254037844387076, 1.000000000000000000, 0.8660254037844387076, 1.000000000000000000, 0.8660254037844387076, 1.000000000000000000, 0.8660254037844387076, 1.000000000000000000, 0.8660254037844387076, 1.000000000000000000, 0.8660254037844387076, 1.000000000000000000, 0.8660254037844387076, 1.000000000000000000, 0.8660254037844387076, 1.000000000000000000, 0.8660254037844387076, 1.000000000000000000, 0.8660254037844387076, 1.000000000000000000, 0.8660254037844387076, 1.000000000000000000, 0.8660254037844387076, 1.000000000000000000, 0.8660254037844387076, 1.000000000000000000, 0.8660254037844387076, 1.000000000000000000, 0.8660254037844387076, 1.000000000000000000, 0.8660254037844387076, 1.000000000000000000, 0.8660254037844387076, 1.000000000000000000, 0.8660254037844387076, 1.000000000000000000, 0.8660254037844387076, 1.000000000000000000, 0.8660254037844387076, 1.000000000000000000, 0.8660254037844387076, 1.000000000000000000, 0.8660254037844387076, 1.000000000000000000, 0.8660254037844387076, 1.000000000000000000, 0.8660254037844387076, 1.000000000000000000, 0.8660254037844387076, 1.000000000000000000, 0.8660254037844387076, 1.000000000000000000, 0.8660254037844387076, 1.000000000000000000, 0.8660254037844387076, 1.000000000000000000, 0.8660254037844387076, 1.000000000000000000, 0.8660254037844387076, 1.000000000000000000, 0.8660254037844387076, 1.000000000000000000, 0.8660254037844387076, 1.000000000000000000, 0.8660254037844387076, 1.000000000000000000, 0.8660254037844387076, 1.000000000000000000, 0.9111410165655264848, 0.9401539157124900736, 0.9401539157124900736, 0.9401539157124900736) ) ) 
 REPRESENTATION_ITEM ( '' )  SURFACE ( )  );
#8772 = CARTESIAN_POINT ( 'NONE',  ( 104.5000000000000142, 12.69999999999998508, 30.20101012677667285 ) ) ;
#8773 = CARTESIAN_POINT ( 'NONE',  ( -79.39999999999999147, -31.03124999877097068, -101.7320508075688821 ) ) ;
#8774 = CARTESIAN_POINT ( 'NONE',  ( 233.9782151781249411, -31.30312499938547788, 97.61286128772489690 ) ) ;
#8775 = CARTESIAN_POINT ( 'NONE',  ( -85.40000000000000568, -33.54374999877096286, 99.99999999999998579 ) ) ;
#8776 = CARTESIAN_POINT ( 'NONE',  ( -79.64356964375001269, -34.49062499938548854, 98.40857419181659793 ) ) ;
#8777 = DIRECTION ( 'NONE',  ( 0.000000000000000000, -1.000000000000000000, 3.597944987211154374E-15 ) ) ;
#8778 = CARTESIAN_POINT ( 'NONE',  ( 229.5999999999999375, -32.21249999999999858, -48.26794919243123161 ) ) ;
#8779 = CARTESIAN_POINT ( 'NONE',  ( 82.39999999999999147, -31.40624999877097068, -96.53589838486223584 ) ) ;
#8780 = CARTESIAN_POINT ( 'NONE',  ( 229.5999999999999375, -34.53749999999999432, 98.26794919243111792 ) ) ;
#8781 = ORIENTED_EDGE ( 'NONE', *, *, #2671, .F. ) ;
#8782 = CARTESIAN_POINT ( 'NONE',  ( 233.4038475772933339, -34.57634618820330275, 97.00000000000000000 ) ) ;
#8783 = CARTESIAN_POINT ( 'NONE',  ( 235.5999999999999375, -33.76874999877096428, 99.99999999999998579 ) ) ;
#8784 = CARTESIAN_POINT ( 'NONE',  ( 229.5999999999999375, -33.05624999877096570, -48.26794919243123161 ) ) ;
#8785 = CARTESIAN_POINT ( 'NONE',  ( -85.15643035625001289, -32.35312499938548569, 101.5914258081833879 ) ) ;
#8786 = ORIENTED_EDGE ( 'NONE', *, *, #12126, .T. ) ;
#8787 = ORIENTED_EDGE ( 'NONE', *, *, #15792, .F. ) ;
#8788 = CARTESIAN_POINT ( 'NONE',  ( -79.39999999999999147, -32.01330983656955453, 99.46005447972481761 ) ) ;
#8789 = CARTESIAN_POINT ( 'NONE',  ( -80.90000000000000568, -34.29374999877096997, 102.5980762113533018 ) ) ;
#8790 = ORIENTED_EDGE ( 'NONE', *, *, #7384, .T. ) ;
#8791 = CARTESIAN_POINT ( 'NONE',  ( -81.28488860390729087, -34.99999999999999289, 102.5271494742948590 ) ) ;
#8792 = CARTESIAN_POINT ( 'NONE',  ( 85.39999999999999147, -34.97364041986484295, -98.90809577818232867 ) ) ;
#8793 = EDGE_CURVE ( 'NONE', #11084, #14672, #84, .T. ) ;
#8794 = FACE_OUTER_BOUND ( 'NONE', #5555, .T. ) ;
#8795 = VECTOR ( 'NONE', #11988, 1000.000000000000000 ) ;
#8796 = VECTOR ( 'NONE', #17888, 1000.000000000000000 ) ;
#8797 = CARTESIAN_POINT ( 'NONE',  ( -83.77821517812500929, -35.12812499938548427, 102.3871387122750889 ) ) ;
#8798 = CARTESIAN_POINT ( 'NONE',  ( -79.39999999999999147, -31.98750000000000071, 98.26794919243110371 ) ) ;
#8799 = CARTESIAN_POINT ( 'NONE',  ( -79.39999999999999147, -31.55624999877096926, 101.7320508075688537 ) ) ;
#8800 = CARTESIAN_POINT ( 'NONE',  ( 82.39999999999999147, -33.43124999877097281, 96.99999999999998579 ) ) ;
#8801 = EDGE_CURVE ( 'NONE', #13499, #16790, #8054, .T. ) ;
#8802 = CARTESIAN_POINT ( 'NONE',  ( 79.69416654173916470, -35.00000000000000711, 99.37250936986644945 ) ) ;
#8803 = CARTESIAN_POINT ( 'NONE',  ( 85.29357727954827340, -35.00000000000000711, 99.68450386720812162 ) ) ;
#8804 = CARTESIAN_POINT ( 'NONE',  ( 231.2217848218749339, -30.21562499938547575, 97.61286128772489690 ) ) ;
#8805 = ORIENTED_EDGE ( 'NONE', *, *, #11373, .F. ) ;
#8806 = CARTESIAN_POINT ( 'NONE',  ( -82.39999999999999147, -34.86562499938548854, -103.1828516163667899 ) ) ;
#8807 = CARTESIAN_POINT ( 'NONE',  ( -85.40000000000000568, -33.56250000000000000, 101.7320508075688821 ) ) ;
#8808 = AXIS2_PLACEMENT_3D ( 'NONE', #8992, #4700, #18182 ) ;
#8809 = AXIS2_PLACEMENT_3D ( 'NONE', #1224, #2781, #14398 ) ;
#8810 = CARTESIAN_POINT ( 'NONE',  ( 233.4038475772933339, -33.91740381056766296, 103.0000000000000000 ) ) ;
#8811 = LINE ( 'NONE', #332, #15529 ) ;
#8812 = CARTESIAN_POINT ( 'NONE',  ( -85.15643035624999868, -35.16562499938547859, 101.5914258081833879 ) ) ;
#8813 = CARTESIAN_POINT ( 'NONE',  ( 79.39999999999999147, -33.37500000000000000, 99.99999999999998579 ) ) ;
#8814 = CARTESIAN_POINT ( 'NONE',  ( 229.8435696437499871, -31.90312499938547575, -48.40857419181671162 ) ) ;
#8815 = VERTEX_POINT ( 'NONE', #14546 ) ;
#8816 = ORIENTED_EDGE ( 'NONE', *, *, #14008, .T. ) ;
#8817 = CARTESIAN_POINT ( 'NONE',  ( 109.9999999999999574, -21.80000000000003268, -139.9999999999999716 ) ) ;
#8818 = CARTESIAN_POINT ( 'NONE',  ( -83.90000000000000568, -32.17500000000000426, 102.5980762113533018 ) ) ;
#8819 = CARTESIAN_POINT ( 'NONE',  ( -80.90000000000000568, -32.04374999877096997, 102.5980762113533018 ) ) ;
#8820 = CARTESIAN_POINT ( 'NONE',  ( 82.39999999999999147, -30.33750000000000213, 96.53589838486223584 ) ) ;
#8821 = DIRECTION ( 'NONE',  ( -1.000000000000000000, 0.000000000000000000, 0.000000000000000000 ) ) ;
#8823 = CARTESIAN_POINT ( 'NONE',  ( 233.9782151781249411, -31.34062499938548285, 102.3871387122750889 ) ) ;
#8822 = VECTOR ( 'NONE', #13277, 1000.000000000000000 ) ;
#8824 = AXIS2_PLACEMENT_3D ( 'NONE', #14988, #1792, #7756 ) ;
#8825 = CARTESIAN_POINT ( 'NONE',  ( 235.3564303562499447, -33.10312499938547859, -48.40857419181671162 ) ) ;
#8826 = CARTESIAN_POINT ( 'NONE',  ( 83.77821517812500929, -34.56562499938548427, 97.61286128772489690 ) ) ;
#8827 = CARTESIAN_POINT ( 'NONE',  ( 83.77821517812500929, -31.86562499938548498, -102.3871387122750889 ) ) ;
#8828 = CARTESIAN_POINT ( 'NONE',  ( 232.5999999999999375, -30.11249999999999716, -53.46410161513786363 ) ) ;
#8829 = CARTESIAN_POINT ( 'NONE',  ( -79.64356964374999848, -34.86562499938548143, 99.99999999999998579 ) ) ;
#8830 = CARTESIAN_POINT ( 'NONE',  ( 79.64356964374999848, -32.16562499938548569, -99.99999999999998579 ) ) ;
#8831 = ORIENTED_EDGE ( 'NONE', *, *, #1956, .T. ) ;
#8832 = CARTESIAN_POINT ( 'NONE',  ( 0.3126073911696408136, 2.020725942163688060, 3.500000000000000000 ) ) ;
#8833 = CARTESIAN_POINT ( 'NONE',  ( 232.5999999999999375, -32.98124999877095576, 102.9999999999999858 ) ) ;
#8834 = CARTESIAN_POINT ( 'NONE',  ( 229.8435696437499871, -30.74062499938547433, -51.59142580818350865 ) ) ;
#8835 = CIRCLE ( 'NONE', #12014, 5.199999999999996625 ) ;
#8836 = CARTESIAN_POINT ( 'NONE',  ( -79.64356964374999848, -32.61562499938548854, 99.99999999999998579 ) ) ;
#8837 = ORIENTED_EDGE ( 'NONE', *, *, #2798, .T. ) ;
#8838 = DIRECTION ( 'NONE',  ( 0.000000000000000000, 0.000000000000000000, 1.000000000000000000 ) ) ;
#8839 = CARTESIAN_POINT ( 'NONE',  ( 231.2217848218749339, -32.76562499938548001, 102.3871387122750889 ) ) ;
#8840 = DIRECTION ( 'NONE',  ( 0.000000000000000000, -0.000000000000000000, -1.000000000000000000 ) ) ;
#8841 = CARTESIAN_POINT ( 'NONE',  ( -83.90000000000000568, -32.62106250001229313, 102.5980762113533018 ) ) ;
#8842 = DIRECTION ( 'NONE',  ( 2.312964634635742582E-14, -1.000000000000000000, 0.000000000000000000 ) ) ;
#8843 = CARTESIAN_POINT ( 'NONE',  ( -85.40000000000000568, -32.25000000000000000, 99.99999999999998579 ) ) ;
#8844 = CARTESIAN_POINT ( 'NONE',  ( -85.15643035625001289, -32.39062499938548711, 99.99999999999998579 ) ) ;
#8845 = CARTESIAN_POINT ( 'NONE',  ( 229.8377951939094714, -35.00000000000000711, 98.91314642826759496 ) ) ;
#8846 = CARTESIAN_POINT ( 'NONE',  ( 85.15643035624999868, -33.44062499938548427, 101.5914258081833879 ) ) ;
#8847 = DIRECTION ( 'NONE',  ( 0.000000000000000000, 0.000000000000000000, 1.000000000000000000 ) ) ;
#8848 = CARTESIAN_POINT ( 'NONE',  ( -82.39999999999999147, -32.58749999999999858, -96.99999999999998579 ) ) ;
#8849 = CARTESIAN_POINT ( 'NONE',  ( -84.44763168836716716, -32.00000000000000000, 101.8452947671445799 ) ) ;
#8850 = CARTESIAN_POINT ( 'NONE',  ( -79.64356964375001269, -30.44062499938548783, -101.5914258081833879 ) ) ;
#8851 = ORIENTED_EDGE ( 'NONE', *, *, #1842, .T. ) ;
#8852 = CARTESIAN_POINT ( 'NONE',  ( 83.90000000000000568, -33.91874999877096997, 97.40192378864668399 ) ) ;
#8853 = DIRECTION ( 'NONE',  ( 0.000000000000000000, -1.000000000000000000, 0.000000000000000000 ) ) ;
#8854 = CARTESIAN_POINT ( 'NONE',  ( 83.20384757729335945, -32.73615380933863150, 102.9999999999999716 ) ) ;
#8855 = ADVANCED_FACE ( 'NONE', ( #7421 ), #4302, .T. ) ;
#8856 = CARTESIAN_POINT ( 'NONE',  ( -85.15643035625001289, -31.15312499938548996, 99.99999999999998579 ) ) ;
#8857 = CARTESIAN_POINT ( 'NONE',  ( 81.90908125320002853, -31.99999999999999289, 102.8381494550125126 ) ) ;
#8858 = ORIENTED_EDGE ( 'NONE', *, *, #4224, .F. ) ;
#8859 = CARTESIAN_POINT ( 'NONE',  ( -85.15643035624999868, -32.87812499938549138, -101.5914258081833879 ) ) ;
#8860 = FACE_OUTER_BOUND ( 'NONE', #17130, .T. ) ;
#8861 = CARTESIAN_POINT ( 'NONE',  ( -85.15643035625001289, -32.50312499938548427, -99.99999999999998579 ) ) ;
#8862 = LINE ( 'NONE', #8772, #7983 ) ;
#8863 = CARTESIAN_POINT ( 'NONE',  ( -83.90000000000000568, -31.36874999877096926, -102.5980762113533018 ) ) ;
#8864 = CARTESIAN_POINT ( 'NONE',  ( 235.3564303562499447, -30.89062499938548001, 98.40857419181659793 ) ) ;
#8865 = CARTESIAN_POINT ( 'NONE',  ( -85.40000000000000568, -30.81018749875867968, 101.7320508075688679 ) ) ;
#8866 = CARTESIAN_POINT ( 'NONE',  ( -79.64356964375001269, -33.14062499938548711, 98.40857419181659793 ) ) ;
#8867 = CARTESIAN_POINT ( 'NONE',  ( -85.15643035625001289, -34.22812499938548569, -101.5914258081833879 ) ) ;
#8868 = CARTESIAN_POINT ( 'NONE',  ( 99.99999999999997158, -5.200000000000008171, -100.0000000000000000 ) ) ;
#8869 = EDGE_CURVE ( 'NONE', #11219, #14097, #2678, .T. ) ;
#8870 = DIRECTION ( 'NONE',  ( 0.000000000000000000, 1.000000000000000000, 0.000000000000000000 ) ) ;
#8871 = CARTESIAN_POINT ( 'NONE',  ( 79.39999999999999147, -33.76874999877097139, -99.99999999999998579 ) ) ;
#8872 = CARTESIAN_POINT ( 'NONE',  ( 235.5999999999999375, -34.27499999999999147, 99.99999999999998579 ) ) ;
#8873 = ORIENTED_EDGE ( 'NONE', *, *, #18365, .T. ) ;
#8874 = CARTESIAN_POINT ( 'NONE',  ( 99.99999999999994316, -29.80000000000000782, 150.0000000000000000 ) ) ;
#8875 = CARTESIAN_POINT ( 'NONE',  ( 233.9782151781249411, -30.40312499938547930, 97.61286128772489690 ) ) ;
#8876 = CARTESIAN_POINT ( 'NONE',  ( 235.5999999999999943, -34.63124999877096144, -51.73205080756900287 ) ) ;
#8877 = EDGE_CURVE ( 'NONE', #3376, #5276, #4203, .T. ) ;
#8878 = CARTESIAN_POINT ( 'NONE',  ( -79.64356964374999848, -34.41562499938548569, 99.99999999999998579 ) ) ;
#8879 = EDGE_LOOP ( 'NONE', ( #1741, #8306 ) ) ;
#8880 = ORIENTED_EDGE ( 'NONE', *, *, #16819, .F. ) ;
#8881 = CARTESIAN_POINT ( 'NONE',  ( -79.39999999999999147, -34.31250000000000000, -98.26794919243113213 ) ) ;
#8882 =( BOUNDED_CURVE ( )  B_SPLINE_CURVE ( 2, ( #2139, #10826, #9556, #18362, #6540, #7706, #15131 ),
 .UNSPECIFIED., .F., .F. ) 
 B_SPLINE_CURVE_WITH_KNOTS ( ( 3, 2, 2, 3 ),
 ( 0.8958333333333333703, 0.9027777777777777901, 0.9166666666666666297, 0.9258785066912882389 ),
 .UNSPECIFIED. ) 
 CURVE ( )  GEOMETRIC_REPRESENTATION_ITEM ( )  RATIONAL_B_SPLINE_CURVE ( ( 0.9330127018922192983, 0.9330127018922198534, 1.000000000000000000, 0.8660254037844387076, 1.000000000000000000, 0.9111410165655264848, 0.9401539157124900736 ) ) 
 REPRESENTATION_ITEM ( '' )  );
#8883 = CARTESIAN_POINT ( 'NONE',  ( 244.7999999999999545, -35.00000000000000000, -100.0000000000000000 ) ) ;
#8884 = CARTESIAN_POINT ( 'NONE',  ( 4.198928548860774157, -0.8158838809860124996, -3.526471437616918170 ) ) ;
#8885 = ORIENTED_EDGE ( 'NONE', *, *, #14777, .F. ) ;
#8886 = CARTESIAN_POINT ( 'NONE',  ( -81.96801452314031167, -35.00000000000000000, 102.7281823352556529 ) ) ;
#8887 = CARTESIAN_POINT ( 'NONE',  ( 229.5999999999999375, -33.99374999877096570, 99.99999999999998579 ) ) ;
#8888 = CARTESIAN_POINT ( 'NONE',  ( -85.15643035624999868, -34.79062499938548569, 98.40857419181659793 ) ) ;
#8889 = CARTESIAN_POINT ( 'NONE',  ( -85.40000000000000568, -34.97364040220742964, 98.90809659374338025 ) ) ;
#8890 = CARTESIAN_POINT ( 'NONE',  ( -79.39999999999999147, -30.61874999877096926, 99.99999999999998579 ) ) ;
#8891 = PLANE ( 'NONE',  #12242 ) ;
#8892 = EDGE_CURVE ( 'NONE', #11060, #14, #14042, .T. ) ;
#8893 = DIRECTION ( 'NONE',  ( -2.312964634635742582E-14, 1.000000000000000000, 0.000000000000000000 ) ) ;
#8894 = CARTESIAN_POINT ( 'NONE',  ( -82.40000000000000568, -34.55624999877097281, -102.9999999999999858 ) ) ;
#8895 = CARTESIAN_POINT ( 'NONE',  ( 235.3564303562499447, -30.81562499938547717, 99.99999999999998579 ) ) ;
#8896 = ORIENTED_EDGE ( 'NONE', *, *, #54, .F. ) ;
#8897 = CARTESIAN_POINT ( 'NONE',  ( -81.02178482187500208, -34.04062499938548569, -97.61286128772489690 ) ) ;
#8898 = CARTESIAN_POINT ( 'NONE',  ( -83.20384757729335945, -33.69240381056766154, 96.99999999999998579 ) ) ;
#8899 = AXIS2_PLACEMENT_3D ( 'NONE', #6712, #8364, #18532 ) ;
#8900 = FACE_OUTER_BOUND ( 'NONE', #18773, .T. ) ;
#8901 = CARTESIAN_POINT ( 'NONE',  ( 231.0999999999999375, -34.51874999877096428, 97.40192378864668399 ) ) ;
#8902 = CARTESIAN_POINT ( 'NONE',  ( -85.15643035625001289, -31.49062499938548498, 99.99999999999998579 ) ) ;
#8903 = FACE_OUTER_BOUND ( 'NONE', #1222, .T. ) ;
#8904 = CARTESIAN_POINT ( 'NONE',  ( 235.3564303562499447, -33.47812499938547148, -51.59142580818350865 ) ) ;
#8905 = VERTEX_POINT ( 'NONE', #16127 ) ;
#8906 = ORIENTED_EDGE ( 'NONE', *, *, #13406, .T. ) ;
#8907 = CARTESIAN_POINT ( 'NONE',  ( -83.90000000000000568, -31.87500000000000000, 97.40192378864668399 ) ) ;
#8908 = EDGE_CURVE ( 'NONE', #17789, #11431, #14646, .T. ) ;
#8909 = CARTESIAN_POINT ( 'NONE',  ( -85.40000000000000568, -31.31250000000000000, 101.7320508075688679 ) ) ;
#8910 = B_SPLINE_CURVE_WITH_KNOTS ( 'NONE', 3,
 ( #11449, #911, #17413, #15942 ),
 .UNSPECIFIED., .F., .F.,
 ( 4, 4 ),
 ( 0.000000000000000000, 0.002452478801916361129 ),
 .UNSPECIFIED. ) ;
#8911 = CARTESIAN_POINT ( 'NONE',  ( -85.40000000000000568, -31.70624999877096784, 101.7320508075688679 ) ) ;
#8912 = CARTESIAN_POINT ( 'NONE',  ( 80.90000000000000568, -33.00000000000000000, 97.40192378864668399 ) ) ;
#8913 = CARTESIAN_POINT ( 'NONE',  ( 85.40000000000000568, -33.54374999877096286, 99.99999999999998579 ) ) ;
#8914 = CARTESIAN_POINT ( 'NONE',  ( 229.8435696437499871, -33.32812499938548001, 98.40857419181659793 ) ) ;
#8915 = AXIS2_PLACEMENT_3D ( 'NONE', #9033, #13523, #14997 ) ;
#8916 = CARTESIAN_POINT ( 'NONE',  ( 229.8435696437499587, -33.32812499938548001, -51.59142580818350154 ) ) ;
#8917 = CARTESIAN_POINT ( 'NONE',  ( 82.39999999999999147, -34.30312499938548143, 103.1828516163667899 ) ) ;
#8918 = CARTESIAN_POINT ( 'NONE',  ( 81.02178482187500208, -30.29062499938548569, -97.61286128772489690 ) ) ;
#8919 = ORIENTED_EDGE ( 'NONE', *, *, #16427, .F. ) ;
#8920 = CARTESIAN_POINT ( 'NONE',  ( 235.5999999999999943, -30.26249999999999218, -48.26794919243124582 ) ) ;
#8921 = CARTESIAN_POINT ( 'NONE',  ( 82.39999999999999147, -34.83749999999999858, -103.0000000000000000 ) ) ;
#8922 = CARTESIAN_POINT ( 'NONE',  ( 85.15643035624999868, -34.15312499938548285, -101.5914258081833879 ) ) ;
#8923 = ORIENTED_EDGE ( 'NONE', *, *, #17119, .T. ) ;
#8924 = CARTESIAN_POINT ( 'NONE',  ( -82.40000000000000568, -30.00000000000000355, -99.99999999999998579 ) ) ;
#8925 = FACE_OUTER_BOUND ( 'NONE', #6348, .T. ) ;
#8926 = CARTESIAN_POINT ( 'NONE',  ( 233.9782151781249411, -31.75312499938547717, -52.38713871227520968 ) ) ;
#8927 = AXIS2_PLACEMENT_3D ( 'NONE', #15610, #9741, #5063 ) ;
#8928 = CARTESIAN_POINT ( 'NONE',  ( -85.40000000000000568, -30.41249999999999787, 101.7320508075688679 ) ) ;
#8929 = EDGE_LOOP ( 'NONE', ( #10000, #1055, #18553, #11594 ) ) ;
#8930 = CARTESIAN_POINT ( 'NONE',  ( -79.39999999999999147, -32.92500000000000426, 99.99999999999998579 ) ) ;
#8931 = CARTESIAN_POINT ( 'NONE',  ( 231.7960411235079050, -35.00000000000002132, 102.6365808225362883 ) ) ;
#8932 = CARTESIAN_POINT ( 'NONE',  ( 79.64356964375001269, -30.32812499938548711, 101.5914258081833879 ) ) ;
#8933 = CARTESIAN_POINT ( 'NONE',  ( -82.39999999999999147, -32.80856250001228602, 96.53589838486223584 ) ) ;
#8934 = CARTESIAN_POINT ( 'NONE',  ( 82.40000000000000568, -30.00000000000000355, 96.99999999999998579 ) ) ;
#8935 = CARTESIAN_POINT ( 'NONE',  ( -82.40000000000001990, -32.13750000000000284, 103.0000000000000000 ) ) ;
#8936 = CARTESIAN_POINT ( 'NONE',  ( -81.02178482187500208, -31.34062499938548996, 102.3871387122750889 ) ) ;
#8937 = CARTESIAN_POINT ( 'NONE',  ( 84.41281071784439405, -31.99999999999999289, 101.8917842577544519 ) ) ;
#8938 = CARTESIAN_POINT ( 'NONE',  ( 79.64356964375001269, -32.69062499938548427, 101.5914258081833879 ) ) ;
#8939 = CARTESIAN_POINT ( 'NONE',  ( 81.59615242270662350, -32.06115380933863435, 96.99999999999997158 ) ) ;
#8940 = CARTESIAN_POINT ( 'NONE',  ( -82.40000000000001990, -33.26250000000000284, 97.00000000000000000 ) ) ;
#8941 = CARTESIAN_POINT ( 'NONE',  ( -84.41281071784422352, -32.00000000000000000, -101.8917842577546651 ) ) ;
#8942 = CARTESIAN_POINT ( 'NONE',  ( -83.77821517812500929, -30.62812499938548783, -97.61286128772489690 ) ) ;
#8943 = ORIENTED_EDGE ( 'NONE', *, *, #7687, .F. ) ;
#8944 = CARTESIAN_POINT ( 'NONE',  ( 79.39999999999999147, -35.11874999877096570, 99.99999999999998579 ) ) ;
#8945=STYLED_ITEM('',(#19350),#3164);
#8946 = CARTESIAN_POINT ( 'NONE',  ( 82.40000000000001990, -33.93750000000000711, -103.0000000000000000 ) ) ;
#8947 = CARTESIAN_POINT ( 'NONE',  ( 85.40000000000000568, -32.64374999877097139, 99.99999999999998579 ) ) ;
#8948 = DIRECTION ( 'NONE',  ( 0.000000000000000000, -1.000000000000000000, 0.000000000000000000 ) ) ;
#8949 = CARTESIAN_POINT ( 'NONE',  ( -81.02178482187500208, -31.75312499938548427, 97.61286128772489690 ) ) ;
#8950 = CARTESIAN_POINT ( 'NONE',  ( 79.39999999999999147, -33.76874999877097139, -99.99999999999998579 ) ) ;
#8951 = EDGE_LOOP ( 'NONE', ( #326, #5297, #18293, #5835, #8124 ) ) ;
#8952 = CARTESIAN_POINT ( 'NONE',  ( -85.40000000000000568, -30.03750000000000497, -101.7320508075688679 ) ) ;
#8953 = CARTESIAN_POINT ( 'NONE',  ( 3.974167765203684866, 0.7238254970431302615, -3.565825589389262085 ) ) ;
#8954 = PLANE ( 'NONE',  #4223 ) ;
#8955 = CARTESIAN_POINT ( 'NONE',  ( -82.39999999999999147, -33.96562499938548285, -103.1828516163667899 ) ) ;
#8956 = DIRECTION ( 'NONE',  ( 0.000000000000000000, -1.000000000000000000, 0.000000000000000000 ) ) ;
#8957 = CARTESIAN_POINT ( 'NONE',  ( -82.39999999999999147, -32.08124999877097139, -96.53589838486223584 ) ) ;
#8958 = EDGE_CURVE ( 'NONE', #15307, #11060, #5040, .T. ) ;
#8959 = CARTESIAN_POINT ( 'NONE',  ( 235.3564303562499447, -32.27812499938548285, 99.99999999999998579 ) ) ;
#8960 = CARTESIAN_POINT ( 'NONE',  ( -85.40000000000000568, -31.71018749875867115, 101.7320508075688679 ) ) ;
#8961 = AXIS2_PLACEMENT_3D ( 'NONE', #13300, #14863, #1588 ) ;
#8962 = B_SPLINE_CURVE_WITH_KNOTS ( 'NONE', 3,
 ( #6667, #9587, #2167, #8123, #12611, #18584 ),
 .UNSPECIFIED., .F., .F.,
 ( 4, 2, 4 ),
 ( 4.336808689942017736E-19, 0.0002095117440864781224, 0.0004190234881729558111 ),
 .UNSPECIFIED. ) ;
#8963 = CARTESIAN_POINT ( 'NONE',  ( -85.15643035624999868, -34.26562499938548711, 101.5914258081833879 ) ) ;
#8964 = CARTESIAN_POINT ( 'NONE',  ( -82.39999999999999147, -31.46249999999999858, 96.99999999999998579 ) ) ;
#8965 = CARTESIAN_POINT ( 'NONE',  ( 82.39999999999999147, -33.62812499938548427, 96.81714838363319586 ) ) ;
#8966 = CARTESIAN_POINT ( 'NONE',  ( -82.39999999999999147, -32.36250000000000426, -102.9999999999999858 ) ) ;
#8967 = DIRECTION ( 'NONE',  ( 0.000000000000000000, 0.000000000000000000, 1.000000000000000000 ) ) ;
#8968 = CARTESIAN_POINT ( 'NONE',  ( 79.39999999999999147, -35.15624999877096712, -101.7320508075688537 ) ) ;
#8969 = VECTOR ( 'NONE', #2179, 1000.000000000000000 ) ;
#8970 = CARTESIAN_POINT ( 'NONE',  ( 235.5999999999999943, -33.33749999999999147, 98.26794919243110371 ) ) ;
#8971 = ORIENTED_EDGE ( 'NONE', *, *, #6864, .T. ) ;
#8972 = CARTESIAN_POINT ( 'NONE',  ( 229.8435696437499303, -33.85312499938548569, -50.00000000000011369 ) ) ;
#8973 =( LENGTH_UNIT ( ) NAMED_UNIT ( * ) SI_UNIT ( .MILLI., .METRE. ) );
#8974 = CARTESIAN_POINT ( 'NONE',  ( 234.0999999999999375, -34.59374999877096002, 97.40192378864668399 ) ) ;
#8975 = CARTESIAN_POINT ( 'NONE',  ( 235.5999999999999943, -33.73124999877096286, -51.73205080756900287 ) ) ;
#8976 = CARTESIAN_POINT ( 'NONE',  ( -79.64356964374998427, -33.92812499938548854, 98.40857419181659793 ) ) ;
#8977 = CIRCLE ( 'NONE', #2121, 5.199999999999996625 ) ;
#8978 = ORIENTED_EDGE ( 'NONE', *, *, #7551, .T. ) ;
#8979 = ORIENTED_EDGE ( 'NONE', *, *, #16774, .T. ) ;
#8980 = CARTESIAN_POINT ( 'NONE',  ( 79.39999999999999147, -34.27499999999999858, -99.99999999999998579 ) ) ;
#8981 = CARTESIAN_POINT ( 'NONE',  ( 111.0000000000000000, 10.19999999999997620, -139.9999999999999716 ) ) ;
#8982 = CARTESIAN_POINT ( 'NONE',  ( 4.114405500665264448, -4.051151509359423031, 2.300149018892232304E-16 ) ) ;
#8983 = ORIENTED_EDGE ( 'NONE', *, *, #16654, .F. ) ;
#8984 = CARTESIAN_POINT ( 'NONE',  ( 79.39999999999999147, -32.41874999877096997, -99.99999999999998579 ) ) ;
#8985 = DIRECTION ( 'NONE',  ( -0.000000000000000000, -0.000000000000000000, -1.000000000000000000 ) ) ;
#8986 = AXIS2_PLACEMENT_3D ( 'NONE', #4643, #19100, #4535 ) ;
#8987 = EDGE_CURVE ( 'NONE', #3780, #5083, #8524, .T. ) ;
#8988 = VECTOR ( 'NONE', #18206, 1000.000000000000000 ) ;
#8989 = CARTESIAN_POINT ( 'NONE',  ( -79.64356964375001269, -33.21562499938548996, 101.5914258081833879 ) ) ;
#8990 = CARTESIAN_POINT ( 'NONE',  ( -79.39999999999999147, -33.82500000000000284, 99.99999999999998579 ) ) ;
#8991 = CARTESIAN_POINT ( 'NONE',  ( -82.39999999999999147, -31.85624999877097352, 96.53589838486223584 ) ) ;
#8992 = CARTESIAN_POINT ( 'NONE',  ( 4.000000000000000000, 2.309401076758497151, -5.000000000000000000 ) ) ;
#8993 = EDGE_CURVE ( 'NONE', #12080, #12231, #6063, .T. ) ;
#8994 = CONICAL_SURFACE ( 'NONE', #11493, 3.500000000000000000, 1.047197551196600296 ) ;
#8995 = CARTESIAN_POINT ( 'NONE',  ( 233.4038475772933339, -33.28259618943232567, 96.99999999999998579 ) ) ;
#8996 = DIRECTION ( 'NONE',  ( -1.000000000000000000, 0.000000000000000000, 0.000000000000000000 ) ) ;
#8997 = CARTESIAN_POINT ( 'NONE',  ( -81.59615242270662350, -34.57634618820329564, -103.0000000000000000 ) ) ;
#8998 = DIRECTION ( 'NONE',  ( 0.000000000000000000, 0.000000000000000000, -1.000000000000000000 ) ) ;
#8999 = VERTEX_POINT ( 'NONE', #12009 ) ;
#9000 = FILL_AREA_STYLE ('',( #1958 ) ) ;
#9001 = CARTESIAN_POINT ( 'NONE',  ( -83.77821517812500929, -32.76562499938548711, -97.61286128772489690 ) ) ;
#9002 = CARTESIAN_POINT ( 'NONE',  ( -82.39999999999999147, -33.48750000000000426, 103.0000000000000000 ) ) ;
#9003 = VECTOR ( 'NONE', #8893, 1000.000000000000000 ) ;
#9004 = CARTESIAN_POINT ( 'NONE',  ( 235.5999999999999943, -34.63124999877096144, -51.73205080756900287 ) ) ;
#9005 = CARTESIAN_POINT ( 'NONE',  ( 81.79008970393682887, -35.00000000000001421, -102.6939647107542299 ) ) ;
#9006 = CARTESIAN_POINT ( 'NONE',  ( -85.15643035624999868, -35.22676555956768141, 98.99674139749697588 ) ) ;
#9007 = DIRECTION ( 'NONE',  ( 0.000000000000000000, 0.000000000000000000, 1.000000000000000000 ) ) ;
#9008 = CARTESIAN_POINT ( 'NONE',  ( 235.3564303562499447, -32.61562499938548143, -50.00000000000011369 ) ) ;
#9010 = EDGE_CURVE ( 'NONE', #17562, #2826, #17597, .T. ) ;
#9009 = ORIENTED_EDGE ( 'NONE', *, *, #3990, .F. ) ;
#9011 = ORIENTED_EDGE ( 'NONE', *, *, #5069, .F. ) ;
#9012 = DIRECTION ( 'NONE',  ( 1.000000000000000000, -4.625929269271494788E-16, 0.000000000000000000 ) ) ;
#9013 = CARTESIAN_POINT ( 'NONE',  ( -85.40000000000000568, -30.93750000000000355, 98.26794919243111792 ) ) ;
#9014 = EDGE_CURVE ( 'NONE', #10754, #8256, #1438, .T. ) ;
#9015 = CARTESIAN_POINT ( 'NONE',  ( -82.39999999999999147, -31.85624999877097352, 96.53589838486223584 ) ) ;
#9016 = CARTESIAN_POINT ( 'NONE',  ( 82.39999999999999147, -31.46250000000000568, 103.4641016151377499 ) ) ;
#9017 = CARTESIAN_POINT ( 'NONE',  ( 111.5000000000000142, 12.69999999999998508, 112.0000000000000142 ) ) ;
#9018 = CARTESIAN_POINT ( 'NONE',  ( 231.2217848218749339, -34.56562499938547717, 102.3871387122750889 ) ) ;
#9019 = CARTESIAN_POINT ( 'NONE',  ( 233.9782151781249411, -34.79062499938547859, -52.38713871227520968 ) ) ;
#9020 = ADVANCED_BREP_SHAPE_REPRESENTATION ( '', ( #7579, #10540 ), #17049 ) ;
#9021 = CARTESIAN_POINT ( 'NONE',  ( 113.0000000000000000, 10.19999999999997264, -145.0000000000000000 ) ) ;
#9022 = CARTESIAN_POINT ( 'NONE',  ( 82.39999999999999147, -30.92812499938548143, -103.1828516163667899 ) ) ;
#9023 = VERTEX_POINT ( 'NONE', #4689 ) ;
#9024 = CARTESIAN_POINT ( 'NONE',  ( 231.0999999999999375, -30.97499999999999432, -52.59807621135342970 ) ) ;
#9025 = CARTESIAN_POINT ( 'NONE',  ( -79.39999999999999147, -31.55624999877096926, 101.7320508075688537 ) ) ;
#9026 = CARTESIAN_POINT ( 'NONE',  ( 82.39999999999999147, -33.40312499938548285, -96.81714838363319586 ) ) ;
#9027 = FACE_OUTER_BOUND ( 'NONE', #18554, .T. ) ;
#9028 = CARTESIAN_POINT ( 'NONE',  ( -83.90000000000000568, -34.81874999877096855, 102.5980762113533018 ) ) ;
#9029 = CARTESIAN_POINT ( 'NONE',  ( -82.39999999999999147, -34.83749999999999858, 103.4641016151377499 ) ) ;
#9030 = CARTESIAN_POINT ( 'NONE',  ( -83.88339518848731302, -35.16733441503058089, 97.47959136244114120 ) ) ;
#9031 = VERTEX_POINT ( 'NONE', #13851 ) ;
#9032 = CARTESIAN_POINT ( 'NONE',  ( 235.3564303562499447, -34.82812499938548001, 98.40857419181659793 ) ) ;
#9033 = CARTESIAN_POINT ( 'NONE',  ( -94.79999999999999716, -5.200000000000000178, 150.0000000000000000 ) ) ;
#9034 = CARTESIAN_POINT ( 'NONE',  ( -80.90000000000000568, -32.09606250001229455, 102.5980762113533018 ) ) ;
#9035 = EDGE_CURVE ( 'NONE', #8383, #5869, #3850, .T. ) ;
#9036 = CARTESIAN_POINT ( 'NONE',  ( -82.40000000000001990, -32.53124999877097423, 103.0000000000000000 ) ) ;
#9037 = CARTESIAN_POINT ( 'NONE',  ( -79.64356964375001269, -31.75312499938548427, 101.5914258081833879 ) ) ;
#9038 = CARTESIAN_POINT ( 'NONE',  ( 229.6750025474186998, -35.00000000000000711, 99.84129707245845964 ) ) ;
#9039 = CARTESIAN_POINT ( 'NONE',  ( 85.15643035625001289, -33.40312499938548285, 99.99999999999998579 ) ) ;
#9040 = DIRECTION ( 'NONE',  ( 1.000000000000000000, 0.000000000000000000, 0.000000000000000000 ) ) ;
#9041 = ADVANCED_FACE ( 'NONE', ( #7614 ), #16673, .F. ) ;
#9042 = CARTESIAN_POINT ( 'NONE',  ( 231.7961524227065979, -33.24240381056766580, -53.00000000000011369 ) ) ;
#9043 = PRODUCT_RELATED_PRODUCT_CATEGORY ( 'part', '', ( #12465 ) ) ;
#9044 = CARTESIAN_POINT ( 'NONE',  ( -84.44763168836720979, -32.00000000000001421, -98.15470523285542015 ) ) ;
#9045 = ORIENTED_EDGE ( 'NONE', *, *, #1723, .T. ) ;
#9046 = CARTESIAN_POINT ( 'NONE',  ( 85.15643035624999868, -30.29062499938548925, 101.5914258081833879 ) ) ;
#9047 = CARTESIAN_POINT ( 'NONE',  ( -0.6507732100473471171, 4.243078065514775510, -0.2236248678334823436 ) ) ;
#9048 = CARTESIAN_POINT ( 'NONE',  ( 113.0000000000000142, 15.19999999999997442, -150.0000000000000000 ) ) ;
#9049 = CARTESIAN_POINT ( 'NONE',  ( -85.15643035624999868, -32.54062499938548569, 98.40857419181659793 ) ) ;
#9050 = CARTESIAN_POINT ( 'NONE',  ( -85.16220480609813137, -35.00000000000002132, -101.0868535717099661 ) ) ;
#9051 = ORIENTED_EDGE ( 'NONE', *, *, #5320, .T. ) ;
#9052 = CARTESIAN_POINT ( 'NONE',  ( -85.40000000000000568, -31.83750000000000568, -101.7320508075688679 ) ) ;
#9053 = CARTESIAN_POINT ( 'NONE',  ( 3.880198502136737115, 0.7307680362927179152, -3.499999999999999556 ) ) ;
#9054 = CARTESIAN_POINT ( 'NONE',  ( 94.79999999999995453, -29.80000000000000071, 150.0000000000000000 ) ) ;
#9055 = CARTESIAN_POINT ( 'NONE',  ( -79.64356964375001269, -34.04062499938549280, -101.5914258081833879 ) ) ;
#9056 = CARTESIAN_POINT ( 'NONE',  ( 82.40000000000000568, -30.00000000000000355, -96.99999999999998579 ) ) ;
#9057 = CARTESIAN_POINT ( 'NONE',  ( 233.9782151781249411, -31.90312499938548285, 102.3871387122750889 ) ) ;
#9058 = CARTESIAN_POINT ( 'NONE',  ( -82.39999999999999147, -32.98518749875867684, 103.4641016151377499 ) ) ;
#9059 = CARTESIAN_POINT ( 'NONE',  ( -83.77821517812500929, -32.42812499938548854, 102.3871387122750889 ) ) ;
#9060 = CARTESIAN_POINT ( 'NONE',  ( 233.4038475772933339, -33.86115380933863150, 102.9999999999999858 ) ) ;
#9061 = CARTESIAN_POINT ( 'NONE',  ( 83.77821517812500929, -34.11562499938548854, 97.61286128772489690 ) ) ;
#9062 = CARTESIAN_POINT ( 'NONE',  ( -96.99999999999998579, -5.200000000000000178, 150.0000000000000000 ) ) ;
#9063 = CYLINDRICAL_SURFACE ( 'NONE', #5844, 3.000000000000002665 ) ;
#9064 = CARTESIAN_POINT ( 'NONE',  ( 85.40000000000000568, -35.30624999877096570, -101.7320508075688679 ) ) ;
#9065 = CARTESIAN_POINT ( 'NONE',  ( 229.5999999999999375, -33.18749999999999289, 98.26794919243111792 ) ) ;
#9066 = ORIENTED_EDGE ( 'NONE', *, *, #12261, .T. ) ;
#9067 = CARTESIAN_POINT ( 'NONE',  ( 232.5999999999999943, -32.61562499938548143, -53.18285161636690361 ) ) ;
#9068 = CARTESIAN_POINT ( 'NONE',  ( 314.9999999999999432, 6.938893903907228378E-15, -150.0000000000001137 ) ) ;
#9069 = CARTESIAN_POINT ( 'NONE',  ( 229.8435696437499871, -31.19062499938548072, 98.40857419181659793 ) ) ;
#9070 = CARTESIAN_POINT ( 'NONE',  ( 232.5999999999999375, -33.20624999877095718, -53.46410161513786363 ) ) ;
#9071 = CARTESIAN_POINT ( 'NONE',  ( -85.15643035625001289, -32.84062499938548285, 99.99999999999998579 ) ) ;
#9072 = EDGE_LOOP ( 'NONE', ( #10952, #2141, #1458, #8013 ) ) ;
#9073 = ORIENTED_EDGE ( 'NONE', *, *, #9358, .F. ) ;
#9074 = CARTESIAN_POINT ( 'NONE',  ( 4.142654963991909689, 2.035398498734317219, -3.525413613457259565 ) ) ;
#9075 = CARTESIAN_POINT ( 'NONE',  ( -82.40000000000000568, -30.00000000000000355, 96.99999999999998579 ) ) ;
#9076 = EDGE_LOOP ( 'NONE', ( #3622, #418, #10965, #6278 ) ) ;
#9077 = DIRECTION ( 'NONE',  ( -0.000000000000000000, -0.000000000000000000, -1.000000000000000000 ) ) ;
#9078 = CARTESIAN_POINT ( 'NONE',  ( 234.0999999999999375, -32.54999999999999716, 102.5980762113533018 ) ) ;
#9079 = CARTESIAN_POINT ( 'NONE',  ( -81.02178482187500208, -34.15312499938548285, 102.3871387122750889 ) ) ;
#9080 = CARTESIAN_POINT ( 'NONE',  ( -80.90000000000000568, -33.45000000000000284, 102.5980762113533018 ) ) ;
#9081 = CARTESIAN_POINT ( 'NONE',  ( -83.90000000000000568, -31.21874999877097068, 102.5980762113533018 ) ) ;
#9082 = LINE ( 'NONE', #12121, #10071 ) ;
#9083 = B_SPLINE_CURVE_WITH_KNOTS ( 'NONE', 3,
 ( #18740, #5459, #11401, #17462 ),
 .UNSPECIFIED., .F., .F.,
 ( 4, 4 ),
 ( 2.380739282167635349E-07, 0.002044882221487541018 ),
 .UNSPECIFIED. ) ;
#9084 = DIRECTION ( 'NONE',  ( 0.000000000000000000, -1.073081856240827827E-16, 1.000000000000000000 ) ) ;
#9085 =( LENGTH_UNIT ( ) NAMED_UNIT ( * ) SI_UNIT ( .MILLI., .METRE. ) );
#9086 = CARTESIAN_POINT ( 'NONE',  ( -81.59615242270662350, -33.46740381056766722, 102.9999999999999716 ) ) ;
#9087 = DIRECTION ( 'NONE',  ( 0.000000000000000000, 0.000000000000000000, -1.000000000000000000 ) ) ;
#9088 = CARTESIAN_POINT ( 'NONE',  ( 229.8435696437499303, -31.94062499938547717, 99.99999999999998579 ) ) ;
#9089 = EDGE_LOOP ( 'NONE', ( #1562, #279, #4202, #4563 ) ) ;
#9090 = SURFACE_SIDE_STYLE ('',( #12129 ) ) ;
#9091 = CARTESIAN_POINT ( 'NONE',  ( -81.02178482187500208, -34.34062499938548285, -102.3871387122750889 ) ) ;
#9092 = CARTESIAN_POINT ( 'NONE',  ( 1.274258131564866448, 3.883108878240963513, -3.220599429844046568 ) ) ;
#9093 = LINE ( 'NONE', #13400, #4597 ) ;
#9094 = CARTESIAN_POINT ( 'NONE',  ( 79.77811200999867935, -34.99999999999999289, -100.8506536761476013 ) ) ;
#9095 = CARTESIAN_POINT ( 'NONE',  ( -83.77821517812500929, -33.66562499938548569, 102.3871387122750889 ) ) ;
#9096 = CARTESIAN_POINT ( 'NONE',  ( 4.000000000000000000, 0.000000000000000000, 0.000000000000000000 ) ) ;
#9097 = CARTESIAN_POINT ( 'NONE',  ( 244.7999999999999545, -4.999999999999976907, 153.0000000000000000 ) ) ;
#9098 = EDGE_CURVE ( 'NONE', #9264, #8145, #10085, .T. ) ;
#9099 = ADVANCED_FACE ( 'NONE', ( #16152, #10291, #19182 ), #3141, .F. ) ;
#9100 = ORIENTED_EDGE ( 'NONE', *, *, #9476, .T. ) ;
#9101 = ORIENTED_EDGE ( 'NONE', *, *, #15736, .T. ) ;
#9102 = DIRECTION ( 'NONE',  ( -0.8191520442889875797, 1.003171929053519570E-16, 0.5735764363510522656 ) ) ;
#9103 = CARTESIAN_POINT ( 'NONE',  ( -79.39999999999999147, -30.63750000000000284, 98.26794919243110371 ) ) ;
#9104 = CARTESIAN_POINT ( 'NONE',  ( -85.40000000000000568, -30.80624999877096926, 101.7320508075688679 ) ) ;
#9105 = CARTESIAN_POINT ( 'NONE',  ( 83.90000000000000568, -30.97500000000000142, 102.5980762113533018 ) ) ;
#9106 = DIRECTION ( 'NONE',  ( 4.625929269271485174E-17, 1.000000000000000000, -0.000000000000000000 ) ) ;
#9107 = CARTESIAN_POINT ( 'NONE',  ( 235.3564303562499447, -34.86562499938547433, 99.99999999999998579 ) ) ;
#9108 = CARTESIAN_POINT ( 'NONE',  ( 85.40000000000000568, -32.23124999877096997, 101.7320508075688821 ) ) ;
#9109 = CARTESIAN_POINT ( 'NONE',  ( 82.85293433256528317, -31.99999999999999289, -97.19890519203640622 ) ) ;
#9110 = VECTOR ( 'NONE', #13072, 1000.000000000000000 ) ;
#9111 = AXIS2_PLACEMENT_3D ( 'NONE', #12706, #2251, #11339 ) ;
#9112 = EDGE_CURVE ( 'NONE', #10812, #11132, #10602, .T. ) ;
#9113 = CARTESIAN_POINT ( 'NONE',  ( 85.15643035625001289, -32.39062499938548711, -99.99999999999998579 ) ) ;
#9114 = ORIENTED_EDGE ( 'NONE', *, *, #7252, .F. ) ;
#9115 = CARTESIAN_POINT ( 'NONE',  ( 232.5999999999999375, -33.03749999999999432, -46.53589838486234953 ) ) ;
#9116 = CARTESIAN_POINT ( 'NONE',  ( -79.64356964374998427, -34.82812499938548711, 98.40857419181659793 ) ) ;
#9117 = CARTESIAN_POINT ( 'NONE',  ( 82.39999999999999147, -32.27812499938548285, -103.1828516163667899 ) ) ;
#9118 = DIRECTION ( 'NONE',  ( 0.000000000000000000, 0.000000000000000000, 1.000000000000000000 ) ) ;
#9119 = FACE_OUTER_BOUND ( 'NONE', #15157, .T. ) ;
#9120 = CARTESIAN_POINT ( 'NONE',  ( 235.3564303562499447, -30.96562499938547930, -48.40857419181671162 ) ) ;
#9121 = CARTESIAN_POINT ( 'NONE',  ( -85.15643035625001289, -35.09062499938548285, 99.99999999999998579 ) ) ;
#9122 = ADVANCED_FACE ( 'NONE', ( #11749 ), #13309, .T. ) ;
#9123 = EDGE_LOOP ( 'NONE', ( #3305, #16935, #18701, #14491 ) ) ;
#9124 = CARTESIAN_POINT ( 'NONE',  ( -85.23110191009446623, -35.00000000000000000, 99.14248198118166044 ) ) ;
#9125 = AXIS2_PLACEMENT_3D ( 'NONE', #7082, #17739, #2391 ) ;
#9126 = CARTESIAN_POINT ( 'NONE',  ( -81.59615242270663771, -31.16115380933863932, 103.0000000000000000 ) ) ;
#9127 = CARTESIAN_POINT ( 'NONE',  ( -79.39999999999999147, -32.51250000000000284, 101.7320508075688537 ) ) ;
#9128 = CARTESIAN_POINT ( 'NONE',  ( -79.39999999999999147, -32.95856250001229881, 101.7320508075688537 ) ) ;
#9129 = CARTESIAN_POINT ( 'NONE',  ( 0.3198814748697593746, 4.434118497892183264, -0.3507732604232499107 ) ) ;
#9130 = CARTESIAN_POINT ( 'NONE',  ( -82.39999999999999147, -31.04062499938548569, 103.1828516163667899 ) ) ;
#9131 = CARTESIAN_POINT ( 'NONE',  ( 111.5000000000000142, 12.69999999999998508, 110.0000000000000142 ) ) ;
#9132 = CARTESIAN_POINT ( 'NONE',  ( 81.02178482187500208, -30.74062499938548498, 102.3871387122750889 ) ) ;
#9133 = LINE ( 'NONE', #1533, #247 ) ;
#9134 = CARTESIAN_POINT ( 'NONE',  ( 229.8435696437499303, -31.49062499938547788, -50.00000000000011369 ) ) ;
#9135 = CARTESIAN_POINT ( 'NONE',  ( -84.82992844608099858, -32.00000000000000000, -101.3134070403134928 ) ) ;
#9136 = CARTESIAN_POINT ( 'NONE',  ( -81.02178482187500208, -32.35312499938548569, -97.61286128772489690 ) ) ;
#9137 = AXIS2_PLACEMENT_3D ( 'NONE', #14062, #16811, #12499 ) ;
#9138 = ORIENTED_EDGE ( 'NONE', *, *, #7100, .T. ) ;
#9139 = CARTESIAN_POINT ( 'NONE',  ( 83.90000000000000568, -35.26874999877097139, 97.40192378864668399 ) ) ;
#9140 = CARTESIAN_POINT ( 'NONE',  ( 83.90000000000000568, -34.51874999877097139, 102.5980762113533018 ) ) ;
#9141 = CARTESIAN_POINT ( 'NONE',  ( -94.79999999999999716, -3.000000000000000000, 150.0000000000000000 ) ) ;
#9142 = CARTESIAN_POINT ( 'NONE',  ( -81.02178482187500208, -32.20312499938548711, 97.61286128772489690 ) ) ;
#9143 = CARTESIAN_POINT ( 'NONE',  ( -1.654252653721913102, -3.663718938583024443, -0.01223254789874440342 ) ) ;
#9144 = ORIENTED_EDGE ( 'NONE', *, *, #2304, .T. ) ;
#9145 = CARTESIAN_POINT ( 'NONE',  ( -82.39999999999999147, -30.56250000000000355, -103.4641016151377499 ) ) ;
#9146 = DIRECTION ( 'NONE',  ( -1.000000000000000000, -0.000000000000000000, -0.000000000000000000 ) ) ;
#9147 = CARTESIAN_POINT ( 'NONE',  ( 82.65333140691205926, -34.99995246259152282, -97.01071553687880566 ) ) ;
#9148 = EDGE_CURVE ( 'NONE', #13062, #4275, #3437, .T. ) ;
#9149 = CARTESIAN_POINT ( 'NONE',  ( -79.64356964375001269, -33.66562499938549280, -98.40857419181659793 ) ) ;
#9150 = CARTESIAN_POINT ( 'NONE',  ( -3.472371940586054251, -2.614027278893156669, -3.320322319202162031 ) ) ;
#9151 = CARTESIAN_POINT ( 'NONE',  ( 232.5999999999999375, -34.41562499938547859, 96.81714838363319586 ) ) ;
#9152 = CARTESIAN_POINT ( 'NONE',  ( -82.39999999999999147, -31.18518749875867968, 103.4641016151377499 ) ) ;
#9153 = ORIENTED_EDGE ( 'NONE', *, *, #16494, .F. ) ;
#9154 = CARTESIAN_POINT ( 'NONE',  ( -81.02178482187500208, -34.45312499938548711, 97.61286128772489690 ) ) ;
#9155 = CARTESIAN_POINT ( 'NONE',  ( -82.40000000000000568, -33.43124999877096570, 102.9999999999999858 ) ) ;
#9156 = CARTESIAN_POINT ( 'NONE',  ( 82.39999999999999147, -33.85312499938548569, 103.1828516163667899 ) ) ;
#9157 = CARTESIAN_POINT ( 'NONE',  ( 0.000000000000000000, 3.755786496842902015E-16, 3.500000000000000000 ) ) ;
#9158 =( BOUNDED_CURVE ( )  B_SPLINE_CURVE ( 2, ( #18094, #8995, #125, #17993, #4704, #10651, #16618, #9474, #6556 ),
 .UNSPECIFIED., .F., .F. ) 
 B_SPLINE_CURVE_WITH_KNOTS ( ( 3, 2, 2, 2, 3 ),
 ( 0.6041666666666667407, 0.6111111111111111605, 0.6250000000000000000, 0.6388888888888888395, 0.6458333333333332593 ),
 .UNSPECIFIED. ) 
 CURVE ( )  GEOMETRIC_REPRESENTATION_ITEM ( )  RATIONAL_B_SPLINE_CURVE ( ( 0.9330127018922192983, 0.9330127018922198534, 1.000000000000000000, 0.8660254037844387076, 1.000000000000000000, 0.8660254037844387076, 1.000000000000000000, 0.9330127018922198534, 0.9330127018922192983 ) ) 
 REPRESENTATION_ITEM ( '' )  );
#9159 = CARTESIAN_POINT ( 'NONE',  ( 233.4038475772932770, -33.22634618820329422, 96.99999999999997158 ) ) ;
#9160 = CARTESIAN_POINT ( 'NONE',  ( 80.90000000000000568, -33.69374999877096855, -97.40192378864668399 ) ) ;
#9161 = CARTESIAN_POINT ( 'NONE',  ( 229.5999999999999375, -32.73749999999999716, 98.26794919243111792 ) ) ;
#9162 = ORIENTED_EDGE ( 'NONE', *, *, #2304, .F. ) ;
#9163 = CARTESIAN_POINT ( 'NONE',  ( 231.2217848218749339, -33.77812499938547575, -47.61286128772501769 ) ) ;
#9164 = DIRECTION ( 'NONE',  ( -1.000000000000000000, -1.336382355046098552E-47, 4.814824860968092260E-31 ) ) ;
#9165 = CARTESIAN_POINT ( 'NONE',  ( 235.3564303562499447, -30.92812499938547788, 99.99999999999998579 ) ) ;
#9166 = CARTESIAN_POINT ( 'NONE',  ( 235.5999999999999375, -35.11874999877095860, -50.00000000000011369 ) ) ;
#9167 = EDGE_CURVE ( 'NONE', #1970, #13473, #16542, .T. ) ;
#9168 = CARTESIAN_POINT ( 'NONE',  ( -82.39999999999999147, -33.40312499938548285, 96.81714838363319586 ) ) ;
#9169 = VERTEX_POINT ( 'NONE', #4423 ) ;
#9170 = ORIENTED_EDGE ( 'NONE', *, *, #17119, .F. ) ;
#9171 = CARTESIAN_POINT ( 'NONE',  ( 4.175075985190094485, 2.060370777630109007, -3.568666869285570531 ) ) ;
#9172 = CARTESIAN_POINT ( 'NONE',  ( 232.5999999999999375, -34.83749999999999147, 103.0000000000000000 ) ) ;
#9173 = CARTESIAN_POINT ( 'NONE',  ( 4.124214193018028496, -4.056676826581953499, 2.739218076410093718E-16 ) ) ;
#9174 = ORIENTED_EDGE ( 'NONE', *, *, #2418, .T. ) ;
#9175 = DIRECTION ( 'NONE',  ( -1.000000000000000000, 0.000000000000000000, 0.000000000000000000 ) ) ;
#9176 = CARTESIAN_POINT ( 'NONE',  ( 235.5999999999999943, -32.51249999999999574, 101.7320508075688537 ) ) ;
#9177 = CARTESIAN_POINT ( 'NONE',  ( -85.15643035624999868, -34.71562499938548285, 101.5914258081833879 ) ) ;
#9178 = CARTESIAN_POINT ( 'NONE',  ( -79.39999999999999147, -34.76250000000000284, 101.7320508075688537 ) ) ;
#9179 = CARTESIAN_POINT ( 'NONE',  ( -82.39999999999999147, -32.75624999877096855, 96.53589838486223584 ) ) ;
#9180 = CYLINDRICAL_SURFACE ( 'NONE', #5098, 3.000000000000002665 ) ;
#9181 = DIRECTION ( 'NONE',  ( 2.407412430484046130E-31, -3.340955887615246502E-46, 1.000000000000000000 ) ) ;
#9182 = DIRECTION ( 'NONE',  ( 1.000000000000000000, 0.000000000000000000, 0.000000000000000000 ) ) ;
#9183 = FACE_OUTER_BOUND ( 'NONE', #11222, .T. ) ;
#9184 = DIRECTION ( 'NONE',  ( -0.000000000000000000, -1.000000000000000000, -0.000000000000000000 ) ) ;
#9185 = CARTESIAN_POINT ( 'NONE',  ( 231.2217848218749339, -32.01562499938548001, 97.61286128772489690 ) ) ;
#9186 = ORIENTED_EDGE ( 'NONE', *, *, #8215, .F. ) ;
#9187 = EDGE_CURVE ( 'NONE', #4798, #15307, #6674, .T. ) ;
#9188 = CARTESIAN_POINT ( 'NONE',  ( -83.77821517812500929, -32.91562499938547859, -102.3871387122750889 ) ) ;
#9189 = CARTESIAN_POINT ( 'NONE',  ( 4.175326769692873086, 4.121399112977848667, 2.543528568011644531E-14 ) ) ;
#9190 = CARTESIAN_POINT ( 'NONE',  ( 234.0999999999999375, -33.89999999999999147, 102.5980762113533018 ) ) ;
#9191 = DIRECTION ( 'NONE',  ( 0.000000000000000000, 1.000000000000000000, 0.000000000000000000 ) ) ;
#9192 = CARTESIAN_POINT ( 'NONE',  ( 229.6750025474185009, -35.00000000000002132, -50.15870292752263282 ) ) ;
#9193 = DIRECTION ( 'NONE',  ( -1.000000000000000000, -0.000000000000000000, -0.000000000000000000 ) ) ;
#9194 = ORIENTED_EDGE ( 'NONE', *, *, #539, .F. ) ;
#9195 = ORIENTED_EDGE ( 'NONE', *, *, #7612, .F. ) ;
#9196 = CARTESIAN_POINT ( 'NONE',  ( -83.09162395290292125, -32.00000000000000711, 102.7516965079135787 ) ) ;
#9197 = CARTESIAN_POINT ( 'NONE',  ( -80.90000000000000568, -30.15000000000000213, 97.40192378864668399 ) ) ;
#9198 = CARTESIAN_POINT ( 'NONE',  ( -85.40000000000000568, -30.84374999877096712, 99.99999999999998579 ) ) ;
#9199 = CARTESIAN_POINT ( 'NONE',  ( 83.90000000000000568, -31.42500000000000071, 102.5980762113533018 ) ) ;
#9200 = PLANE ( 'NONE',  #19294 ) ;
#9201 = CARTESIAN_POINT ( 'NONE',  ( 229.8435696437499871, -32.87812499938547717, 98.40857419181659793 ) ) ;
#9202 = CARTESIAN_POINT ( 'NONE',  ( 85.15643035625001289, -32.95312499938548711, -99.99999999999998579 ) ) ;
#9203 = CARTESIAN_POINT ( 'NONE',  ( 82.40000000000000568, -30.00000000000000355, 99.99999999999998579 ) ) ;
#9204 = CARTESIAN_POINT ( 'NONE',  ( 81.02178482187500208, -34.94062499938548427, -102.3871387122750889 ) ) ;
#9205 = VERTEX_POINT ( 'NONE', #5990 ) ;
#9206 = CARTESIAN_POINT ( 'NONE',  ( 229.5999999999999375, -33.60000000000000142, -50.00000000000011369 ) ) ;
#9207 = CARTESIAN_POINT ( 'NONE',  ( 83.77821517812500929, -32.91562499938547859, -97.61286128772489690 ) ) ;
#9208 = CARTESIAN_POINT ( 'NONE',  ( 79.64356964375001269, -32.65312499938548285, -101.5914258081833879 ) ) ;
#9209 = DIRECTION ( 'NONE',  ( 0.000000000000000000, -1.000000000000000000, 0.000000000000000000 ) ) ;
#9210 = CARTESIAN_POINT ( 'NONE',  ( -81.02178482187500208, -31.90312499938548996, 102.3871387122750889 ) ) ;
#9211 = CARTESIAN_POINT ( 'NONE',  ( 233.9782151781249411, -34.00312499938547717, -52.38713871227520968 ) ) ;
#9212 = CARTESIAN_POINT ( 'NONE',  ( -80.90000000000000568, -30.60000000000000142, 97.40192378864668399 ) ) ;
#9213 = ORIENTED_EDGE ( 'NONE', *, *, #14147, .T. ) ;
#9214 = CARTESIAN_POINT ( 'NONE',  ( -83.66537704785669405, -35.00036927961398447, 102.7253295689626782 ) ) ;
#9215 = ADVANCED_FACE ( 'NONE', ( #13210 ), #17912, .F. ) ;
#9216 = AXIS2_PLACEMENT_3D ( 'NONE', #6818, #5638, #16079 ) ;
#9217 = CARTESIAN_POINT ( 'NONE',  ( 229.8435696437499303, -34.64062499938548001, 99.99999999999998579 ) ) ;
#9218 = CARTESIAN_POINT ( 'NONE',  ( 83.77821517812500929, -30.51562499938548711, 97.61286128772489690 ) ) ;
#9219 =( BOUNDED_CURVE ( )  B_SPLINE_CURVE ( 2, ( #6773, #18493, #11054, #2072, #16928, #9494, #9395, #2358, #3633 ),
 .UNSPECIFIED., .F., .F. ) 
 B_SPLINE_CURVE_WITH_KNOTS ( ( 3, 2, 2, 2, 3 ),
 ( 0.5208333333333334814, 0.5277777777777777901, 0.5416666666666666297, 0.5555555555555555802, 0.5625000000000000000 ),
 .UNSPECIFIED. ) 
 CURVE ( )  GEOMETRIC_REPRESENTATION_ITEM ( )  RATIONAL_B_SPLINE_CURVE ( ( 0.9330127018922194093, 0.9330127018922209636, 1.000000000000000000, 0.8660254037844387076, 1.000000000000000000, 0.8660254037844387076, 1.000000000000000000, 0.9330127018922194093, 0.9330127018922194093 ) ) 
 REPRESENTATION_ITEM ( '' )  );
#9220 = CARTESIAN_POINT ( 'NONE',  ( 230.5523683116323355, -32.00000000000000000, -48.15470523285603832 ) ) ;
#9221 = CARTESIAN_POINT ( 'NONE',  ( -82.39999999999999147, -32.16562499938548569, 96.81714838363319586 ) ) ;
#9222 = CARTESIAN_POINT ( 'NONE',  ( -79.39999999999999147, -32.43750000000000000, 98.26794919243110371 ) ) ;
#9223 = CARTESIAN_POINT ( 'NONE',  ( 83.77821517812500929, -34.82812499938548711, 102.3871387122750889 ) ) ;
#9224 = EDGE_CURVE ( 'NONE', #16242, #2738, #2909, .T. ) ;
#9225 = CARTESIAN_POINT ( 'NONE',  ( 81.02178482187500208, -31.30312499938548498, -97.61286128772489690 ) ) ;
#9226 = CARTESIAN_POINT ( 'NONE',  ( 231.2217848218749339, -30.66562499938547859, -52.38713871227520968 ) ) ;
#9227 = CARTESIAN_POINT ( 'NONE',  ( -85.03799702444354125, -32.00000000000001421, -100.8187845449568130 ) ) ;
#9228 = CARTESIAN_POINT ( 'NONE',  ( -83.77821517812500929, -34.82812499938548711, -102.3871387122750889 ) ) ;
#9229 = CIRCLE ( 'NONE', #17362, 3.000000000000002665 ) ;
#9230 = PRODUCT_DEFINITION_CONTEXT ( 'detailed design', #7950, 'design' ) ;
#9231 = EDGE_LOOP ( 'NONE', ( #1130, #11631, #16100, #14383 ) ) ;
#9232 = CARTESIAN_POINT ( 'NONE',  ( 82.39999999999999147, -35.23124999877096997, 96.53589838486223584 ) ) ;
#9233 = CARTESIAN_POINT ( 'NONE',  ( -83.90000000000000568, -33.16874999877096286, 97.40192378864668399 ) ) ;
#9234 = DIRECTION ( 'NONE',  ( -0.000000000000000000, -1.000000000000000000, -0.000000000000000000 ) ) ;
#9235 = CARTESIAN_POINT ( 'NONE',  ( -81.02178482187500208, -32.65312499938548996, 97.61286128772489690 ) ) ;
#9236 = CARTESIAN_POINT ( 'NONE',  ( -82.40000000000000568, -30.00000000000000355, 99.99999999999998579 ) ) ;
#9237 = ORIENTED_EDGE ( 'NONE', *, *, #9865, .T. ) ;
#9238 = EDGE_CURVE ( 'NONE', #3130, #4798, #15968, .T. ) ;
#9239 = CARTESIAN_POINT ( 'NONE',  ( -83.90000000000000568, -31.72500000000000142, -97.40192378864668399 ) ) ;
#9240 = EDGE_CURVE ( 'NONE', #4006, #5317, #17425, .T. ) ;
#9241 = CARTESIAN_POINT ( 'NONE',  ( 85.40000000000000568, -34.01250000000000284, -101.7320508075688679 ) ) ;
#9242 = DIRECTION ( 'NONE',  ( 0.000000000000000000, 1.000000000000000000, -1.073081856240829182E-16 ) ) ;
#9243 = LINE ( 'NONE', #18437, #12353 ) ;
#9244 = EDGE_CURVE ( 'NONE', #6950, #15931, #10674, .T. ) ;
#9245 = DIRECTION ( 'NONE',  ( 4.625929269271494788E-16, 1.000000000000000000, -0.000000000000000000 ) ) ;
#9246 = CARTESIAN_POINT ( 'NONE',  ( 235.3564303562499447, -34.07812499938548001, 99.99999999999998579 ) ) ;
#9247 = CARTESIAN_POINT ( 'NONE',  ( -80.90000000000000568, -30.99768749875867968, 97.40192378864668399 ) ) ;
#9248 = VERTEX_POINT ( 'NONE', #1875 ) ;
#9249 = CARTESIAN_POINT ( 'NONE',  ( 105.1999999999999886, -34.99999999999999289, -97.80000000000002558 ) ) ;
#9250 = CARTESIAN_POINT ( 'NONE',  ( 0.000000000000000000, 0.000000000000000000, -5.000000000000000888 ) ) ;
#9251 = CARTESIAN_POINT ( 'NONE',  ( 81.02178482187500208, -33.44062499938548427, 102.3871387122750889 ) ) ;
#9252 = CARTESIAN_POINT ( 'NONE',  ( 80.90000000000000568, -34.20000000000000284, 102.5980762113533018 ) ) ;
#9253 = CARTESIAN_POINT ( 'NONE',  ( 234.0999999999999375, -33.24374999877096570, 97.40192378864668399 ) ) ;
#9254 = CARTESIAN_POINT ( 'NONE',  ( 82.39999999999999147, -34.33124999877097139, -103.4641016151377499 ) ) ;
#9255 = CARTESIAN_POINT ( 'NONE',  ( 82.40000000000000568, -34.78124999877096712, 96.99999999999998579 ) ) ;
#9256 = CARTESIAN_POINT ( 'NONE',  ( -79.64356964374999848, -33.06562499938548427, -99.99999999999998579 ) ) ;
#9257 = ORIENTED_EDGE ( 'NONE', *, *, #11545, .T. ) ;
#9258 = CARTESIAN_POINT ( 'NONE',  ( 229.8435696437499303, -32.50312499938547717, -50.00000000000011369 ) ) ;
#9259 = ADVANCED_FACE ( 'NONE', ( #13697 ), #7929, .T. ) ;
#9260 = CARTESIAN_POINT ( 'NONE',  ( 235.5999999999999375, -35.11874999877095860, 99.99999999999998579 ) ) ;
#9261 = CARTESIAN_POINT ( 'NONE',  ( 233.9782151781249411, -31.45312499938548356, -47.61286128772501769 ) ) ;
#9262 = VECTOR ( 'NONE', #7695, 1000.000000000000000 ) ;
#9263 = CARTESIAN_POINT ( 'NONE',  ( -85.15643035625001289, -34.67812499938548143, 98.40857419181659793 ) ) ;
#9264 = VERTEX_POINT ( 'NONE', #9488 ) ;
#9265 = ORIENTED_EDGE ( 'NONE', *, *, #1048, .T. ) ;
#9266 = CARTESIAN_POINT ( 'NONE',  ( -83.77821517812500929, -30.21562499938548285, -102.3871387122750889 ) ) ;
#9267 = CARTESIAN_POINT ( 'NONE',  ( 232.5999999999999091, -33.03749999999998721, 102.9999999999999858 ) ) ;
#9268 = CARTESIAN_POINT ( 'NONE',  ( -85.40000000000000568, -34.01250000000000284, -98.26794919243111792 ) ) ;
#9269 = ORIENTED_EDGE ( 'NONE', *, *, #13688, .T. ) ;
#9270 = CARTESIAN_POINT ( 'NONE',  ( 105.1999999999999744, -31.99999999999999289, -100.0000000000000000 ) ) ;
#9271 = CARTESIAN_POINT ( 'NONE',  ( -81.59615242270662350, -33.91740381056766296, 103.0000000000000000 ) ) ;
#9272 = CARTESIAN_POINT ( 'NONE',  ( -83.90000000000000568, -33.52499999999999858, 102.5980762113533018 ) ) ;
#9273 =( BOUNDED_CURVE ( )  B_SPLINE_CURVE ( 2, ( #11722, #12999, #17500, #13383, #7042, #17, #3023, #11823, #17792 ),
 .UNSPECIFIED., .F., .F. ) 
 B_SPLINE_CURVE_WITH_KNOTS ( ( 3, 2, 2, 2, 3 ),
 ( 0.3125000000000001665, 0.3194444444444444198, 0.3333333333333333148, 0.3472222222222222099, 0.3541666666666666297 ),
 .UNSPECIFIED. ) 
 CURVE ( )  GEOMETRIC_REPRESENTATION_ITEM ( )  RATIONAL_B_SPLINE_CURVE ( ( 0.9330127018922194093, 0.9330127018922209636, 1.000000000000000000, 0.8660254037844387076, 1.000000000000000000, 0.8660254037844387076, 1.000000000000000000, 0.9330127018922196314, 0.9330127018922194093 ) ) 
 REPRESENTATION_ITEM ( '' )  );
#9274 = EDGE_CURVE ( 'NONE', #13854, #2849, #2065, .T. ) ;
#9275 = CARTESIAN_POINT ( 'NONE',  ( -79.39999999999999147, -33.76874999877097139, 99.99999999999998579 ) ) ;
#9276 = VECTOR ( 'NONE', #6220, 1000.000000000000000 ) ;
#9277 = CARTESIAN_POINT ( 'NONE',  ( 232.5999999999999375, -32.36249999999999716, 97.00000000000000000 ) ) ;
#9278 = CARTESIAN_POINT ( 'NONE',  ( -82.40000000000000568, -33.71249999999998437, 96.99999999999998579 ) ) ;
#9279 = DIRECTION ( 'NONE',  ( 0.000000000000000000, -1.000000000000000000, 0.000000000000000000 ) ) ;
#9280 = CARTESIAN_POINT ( 'NONE',  ( 4.052424581287662697, 3.786734753435040179, 0.5771415817957487038 ) ) ;
#9281 = DIRECTION ( 'NONE',  ( -0.000000000000000000, -1.000000000000000000, -0.000000000000000000 ) ) ;
#9282 = CARTESIAN_POINT ( 'NONE',  ( 229.8435696437499871, -32.35312499938547859, 101.5914258081833879 ) ) ;
#9283 = ORIENTED_EDGE ( 'NONE', *, *, #18203, .F. ) ;
#9284 = CARTESIAN_POINT ( 'NONE',  ( -85.15643035624999868, -33.70312499938548711, -98.40857419181659793 ) ) ;
#9285 = CARTESIAN_POINT ( 'NONE',  ( 4.165266963751924401, 4.099263933823841910, -9.393296756667078455E-16 ) ) ;
#9286 = ORIENTED_EDGE ( 'NONE', *, *, #2917, .T. ) ;
#9287 = FACE_OUTER_BOUND ( 'NONE', #13472, .T. ) ;
#9288 = CARTESIAN_POINT ( 'NONE',  ( 83.03192786677293213, -35.00000000000000000, -102.6890373435400221 ) ) ;
#9289 = CARTESIAN_POINT ( 'NONE',  ( 232.5999999999999375, -29.99999999999999645, -50.00000000000011369 ) ) ;
#9290 = CARTESIAN_POINT ( 'NONE',  ( 230.4884518427504076, -35.14114861271050216, -51.77179927996177611 ) ) ;
#9291 = CONICAL_SURFACE ( 'NONE', #12422, 4.000000000000000000, 0.8911886515913786111 ) ;
#9292 = VECTOR ( 'NONE', #14479, 1000.000000000000000 ) ;
#9293 = EDGE_LOOP ( 'NONE', ( #16622, #2707, #13564, #17393 ) ) ;
#9294 = ORIENTED_EDGE ( 'NONE', *, *, #6043, .T. ) ;
#9295 = CARTESIAN_POINT ( 'NONE',  ( 232.5999999999999375, -29.99999999999999645, -50.00000000000011369 ) ) ;
#9296 = CARTESIAN_POINT ( 'NONE',  ( 80.90000000000000568, -31.20000000000000284, -102.5980762113533018 ) ) ;
#9297 = CARTESIAN_POINT ( 'NONE',  ( -82.39999999999999147, -33.43124999877097281, 103.4641016151377499 ) ) ;
#9298 = CARTESIAN_POINT ( 'NONE',  ( 79.39999999999999147, -32.92500000000000426, 99.99999999999998579 ) ) ;
#9299 = CIRCLE ( 'NONE', #1807, 7.500000000000020428 ) ;
#9300 = CARTESIAN_POINT ( 'NONE',  ( -79.79666399293490997, -31.99999999999999289, -98.51078102784448731 ) ) ;
#9301 = CARTESIAN_POINT ( 'NONE',  ( 233.9782151781249411, -32.99062499938548143, 97.61286128772489690 ) ) ;
#9302 = CARTESIAN_POINT ( 'NONE',  ( 79.64356964374999848, -33.17812499938548854, -99.99999999999998579 ) ) ;
#9303 = VECTOR ( 'NONE', #6776, 1000.000000000000000 ) ;
#9304 = DIRECTION ( 'NONE',  ( 1.000000000000000000, 0.000000000000000000, -0.000000000000000000 ) ) ;
#9305 =( BOUNDED_CURVE ( )  B_SPLINE_CURVE ( 2, ( #8458, #12956, #14321, #18927, #12864, #11496, #5642, #7098, #13055 ),
 .UNSPECIFIED., .F., .F. ) 
 B_SPLINE_CURVE_WITH_KNOTS ( ( 3, 2, 2, 2, 3 ),
 ( 0.6458333333333332593, 0.6527777777777777901, 0.6666666666666666297, 0.6805555555555555802, 0.6875000000000000000 ),
 .UNSPECIFIED. ) 
 CURVE ( )  GEOMETRIC_REPRESENTATION_ITEM ( )  RATIONAL_B_SPLINE_CURVE ( ( 0.9330127018922192983, 0.9330127018922187432, 1.000000000000000000, 0.8660254037844387076, 1.000000000000000000, 0.8660254037844387076, 1.000000000000000000, 0.9330127018922194093, 0.9330127018922194093 ) ) 
 REPRESENTATION_ITEM ( '' )  );
#9306 = CARTESIAN_POINT ( 'NONE',  ( 85.15643035624999868, -34.15312499938548285, -101.5914258081833879 ) ) ;
#9307 = ORIENTED_EDGE ( 'NONE', *, *, #16365, .F. ) ;
#9308 = CARTESIAN_POINT ( 'NONE',  ( 232.5999999999999375, -31.46249999999999858, -53.46410161513786363 ) ) ;
#9309 = CARTESIAN_POINT ( 'NONE',  ( -79.39999999999999147, -34.68750000000000000, 98.26794919243110371 ) ) ;
#9310 = CARTESIAN_POINT ( 'NONE',  ( -85.40000000000000568, -30.86250000000000071, 101.7320508075688821 ) ) ;
#9311 = CARTESIAN_POINT ( 'NONE',  ( 83.90000000000000568, -33.67500000000000426, 102.5980762113533018 ) ) ;
#9312 = CARTESIAN_POINT ( 'NONE',  ( -82.39999999999999147, -30.36562499938549209, 96.81714838363319586 ) ) ;
#9313 = CARTESIAN_POINT ( 'NONE',  ( 229.8435696437499871, -34.34062499938547575, -51.59142580818350865 ) ) ;
#9314 = CARTESIAN_POINT ( 'NONE',  ( -79.64356964375001269, -34.82812499938548711, 98.40857419181659793 ) ) ;
#9315 = VERTEX_POINT ( 'NONE', #12517 ) ;
#9316 = CARTESIAN_POINT ( 'NONE',  ( -85.40074734447198068, -35.00045574454757968, 100.3204239692404371 ) ) ;
#9317 = CARTESIAN_POINT ( 'NONE',  ( -79.39999999999999147, -34.23750000000000426, 98.26794919243110371 ) ) ;
#9318 = FACE_BOUND ( 'NONE', #12305, .T. ) ;
#9319 = CARTESIAN_POINT ( 'NONE',  ( 232.5999999999999375, -34.61249999999999716, 97.00000000000000000 ) ) ;
#9320 = CARTESIAN_POINT ( 'NONE',  ( -81.02178482187500208, -31.90312499938548996, 102.3871387122750889 ) ) ;
#9321 = CARTESIAN_POINT ( 'NONE',  ( -94.79999999999999716, -5.200000000000000178, -150.0000000000000000 ) ) ;
#9322 = CARTESIAN_POINT ( 'NONE',  ( 85.15643035624999868, -31.00312499938548072, 98.40857419181659793 ) ) ;
#9323 = CARTESIAN_POINT ( 'NONE',  ( 85.15643035624999868, -31.19062499938548783, -98.40857419181659793 ) ) ;
#9324 = CARTESIAN_POINT ( 'NONE',  ( 232.5999999999999375, -31.82812499938547290, -46.81714838363331666 ) ) ;
#9325 = CARTESIAN_POINT ( 'NONE',  ( -82.39999999999999147, -34.86562499938548854, 96.81714838363319586 ) ) ;
#9326 = CARTESIAN_POINT ( 'NONE',  ( -85.15643035625001289, -32.95312499938548711, -99.99999999999998579 ) ) ;
#9327 = ORIENTED_EDGE ( 'NONE', *, *, #3012, .F. ) ;
#9328 = CARTESIAN_POINT ( 'NONE',  ( 82.39999999999999147, -31.04062499938548569, 96.81714838363319586 ) ) ;
#9329 = LINE ( 'NONE', #10705, #12097 ) ;
#9330 =( LENGTH_UNIT ( ) NAMED_UNIT ( * ) SI_UNIT ( .MILLI., .METRE. ) );
#9331 = CARTESIAN_POINT ( 'NONE',  ( -85.15643035624999868, -32.99062499938548854, 98.40857419181659793 ) ) ;
#9332 = CARTESIAN_POINT ( 'NONE',  ( 235.5999999999999943, -32.06249999999999289, -48.26794919243124582 ) ) ;
#9333 = ORIENTED_EDGE ( 'NONE', *, *, #3518, .T. ) ;
#9334 = CARTESIAN_POINT ( 'NONE',  ( -83.90000000000000568, -31.27500000000000568, -97.40192378864668399 ) ) ;
#9335 = EDGE_CURVE ( 'NONE', #7020, #5172, #18487, .T. ) ;
#9336 =( BOUNDED_SURFACE ( )  B_SPLINE_SURFACE ( 1, 2, ( 
 ( #11692, #11315, #8761, #14713, #15812, #1351, #12873, #18144, #13537, #7779, #12078, #2901, #17763, #1437, #16291, #15106, #18055, #4466, #16672, #7492, #11793, #4766, #83, #1720, #8856, #7587, #14811, #11983, #179, #12176, #10420, #16384, #2993, #277, #5840, #10518, #3183, #11884, #7392, #14917, #8949, #10707, #1633, #1544, #3278, #4370, #6128, #13355, #13447, #13305, #16486, #5937, #9142, #17855, #10614, #7678, #6034, #15199, #17951, #4561, #3088, #9049, #4664, #13632, #9235, #15013, #16580, #6228, #1817, #13733, #10329, #5244, #10899, #9331, #18430, #9531, #3382, #2109, #12557, #8166, #560, #2297, #15296, #5142, #14115, #12370, #16866, #5049, #14024, #13824, #18526, #12654, #10801, #3472, #8070, #18239, #18336, #18626, #8262, #6414, #15398, #9432, #659, #4957, #2008, #15693, #11089, #7968, #13922, #752, #372, #6518, #12460, #10994, #6324, #17058, #16960, #11193, #16765, #17156, #3764, #3571, #9729, #6607, #6707, #12276, #15597, #9636, #3671, #4857, #466, #1909, #7873, #15496, #2205 ),
 ( #17450, #8545, #9824, #17542, #15788, #11287, #18824, #5446, #6994, #10021, #19013, #12852, #4061, #1041, #11484, #9926, #2395, #5633, #949, #17257, #15887, #14402, #3862, #12945, #15980, #14496, #17350, #10118, #5347, #2584, #1129, #8357, #6904, #2492, #18917, #14311, #7086, #13042, #18726, #11384, #5536, #6811, #3960, #11579, #16073, #8450, #4160, #14211, #848, #12757, #2077, #8324, #17128, #630, #18402, #819, #916, #3543, #5022, #9499, #14280, #9698, #11058, #3825, #3446, #5315, #9795, #10963, #15756, #14087, #6777, #2363, #8235, #2267, #18595, #11256, #12434, #12338, #18304, #15660, #14183, #17220, #725, #4924, #5212, #9401, #10869, #7938, #15363, #12727, #11159, #16931, #16840, #13991, #1981, #13889, #6578, #18699, #527, #6680, #6482, #18497, #12623, #15466, #8033, #12526, #5118, #17028, #3639, #9601, #15565, #2178, #8135, #3733, #9991, #13197, #2642, #17419, #5781, #18786, #1196, #12916, #14660, #14758, #5605, #12821, #16139, #1295, #13103, #4031, #18884, #15947, #5506, #11453, #6874 ) ),
 .UNSPECIFIED., .F., .F., .F. ) 
 B_SPLINE_SURFACE_WITH_KNOTS ( ( 2, 2 ),
 ( 3, 2, 2, 2, 2, 2, 2, 2, 2, 2, 2, 2, 2, 2, 2, 2, 2, 2, 2, 2, 2, 2, 2, 2, 2, 2, 2, 2, 2, 2, 2, 2, 2, 2, 2, 2, 2, 2, 2, 2, 2, 2, 2, 2, 2, 2, 2, 2, 2, 2, 2, 2, 2, 2, 2, 2, 2, 2, 2, 2, 2, 2, 2, 2, 2, 2, 2, 3 ),
 ( 0.000000000000000000, 1.000000000000000000 ),
 ( 0.000000000000000000, 0.01388888888888888812, 0.02777777777777777624, 0.04166666666666666435, 0.05555555555555555247, 0.06944444444444444753, 0.08333333333333332871, 0.09722222222222222376, 0.1111111111111111049, 0.1250000000000000000, 0.1388888888888888951, 0.1527777777777777901, 0.1666666666666666574, 0.1805555555555555525, 0.1944444444444444475, 0.2083333333333333426, 0.2222222222222222099, 0.2361111111111111049, 0.2500000000000000000, 0.2638888888888888951, 0.2777777777777777901, 0.2916666666666666852, 0.3055555555555555802, 0.3194444444444444198, 0.3333333333333333148, 0.3472222222222222099, 0.3611111111111111049, 0.3750000000000000000, 0.3888888888888888951, 0.4027777777777777901, 0.4166666666666666852, 0.4305555555555555802, 0.4444444444444444198, 0.4583333333333333148, 0.4722222222222222099, 0.4861111111111111049, 0.5000000000000000000, 0.5138888888888888395, 0.5277777777777777901, 0.5416666666666666297, 0.5555555555555555802, 0.5694444444444444198, 0.5833333333333333703, 0.5972222222222222099, 0.6111111111111111605, 0.6250000000000000000, 0.6388888888888888395, 0.6527777777777777901, 0.6666666666666666297, 0.6805555555555555802, 0.6944444444444444198, 0.7083333333333333703, 0.7222222222222222099, 0.7361111111111111605, 0.7500000000000000000, 0.7638888888888888395, 0.7777777777777777901, 0.7916666666666666297, 0.8055555555555555802, 0.8194444444444444198, 0.8333333333333333703, 0.8472222222222222099, 0.8611111111111111605, 0.8750000000000000000, 0.8888888888888888395, 0.9027777777777777901, 0.9166666666666666297, 0.9258785565094813652 ),
 .UNSPECIFIED. ) 
 GEOMETRIC_REPRESENTATION_ITEM ( )  RATIONAL_B_SPLINE_SURFACE ( (
 ( 1.000000000000000000, 0.8660254037844387076, 1.000000000000000000, 0.8660254037844387076, 1.000000000000000000, 0.8660254037844387076, 1.000000000000000000, 0.8660254037844387076, 1.000000000000000000, 0.8660254037844387076, 1.000000000000000000, 0.8660254037844387076, 1.000000000000000000, 0.8660254037844387076, 1.000000000000000000, 0.8660254037844387076, 1.000000000000000000, 0.8660254037844387076, 1.000000000000000000, 0.8660254037844387076, 1.000000000000000000, 0.8660254037844387076, 1.000000000000000000, 0.8660254037844387076, 1.000000000000000000, 0.8660254037844387076, 1.000000000000000000, 0.8660254037844387076, 1.000000000000000000, 0.8660254037844387076, 1.000000000000000000, 0.8660254037844387076, 1.000000000000000000, 0.8660254037844387076, 1.000000000000000000, 0.8660254037844387076, 1.000000000000000000, 0.8660254037844387076, 1.000000000000000000, 0.8660254037844387076, 1.000000000000000000, 0.8660254037844387076, 1.000000000000000000, 0.8660254037844387076, 1.000000000000000000, 0.8660254037844387076, 1.000000000000000000, 0.8660254037844387076, 1.000000000000000000, 0.8660254037844387076, 1.000000000000000000, 0.8660254037844387076, 1.000000000000000000, 0.8660254037844387076, 1.000000000000000000, 0.8660254037844387076, 1.000000000000000000, 0.8660254037844387076, 1.000000000000000000, 0.8660254037844387076, 1.000000000000000000, 0.8660254037844387076, 1.000000000000000000, 0.8660254037844387076, 1.000000000000000000, 0.8660254037844387076, 1.000000000000000000, 0.8660254037844387076, 1.000000000000000000, 0.8660254037844387076, 1.000000000000000000, 0.8660254037844387076, 1.000000000000000000, 0.8660254037844387076, 1.000000000000000000, 0.8660254037844387076, 1.000000000000000000, 0.8660254037844387076, 1.000000000000000000, 0.8660254037844387076, 1.000000000000000000, 0.8660254037844387076, 1.000000000000000000, 0.8660254037844387076, 1.000000000000000000, 0.8660254037844387076, 1.000000000000000000, 0.8660254037844387076, 1.000000000000000000, 0.8660254037844387076, 1.000000000000000000, 0.8660254037844387076, 1.000000000000000000, 0.8660254037844387076, 1.000000000000000000, 0.8660254037844387076, 1.000000000000000000, 0.8660254037844387076, 1.000000000000000000, 0.8660254037844387076, 1.000000000000000000, 0.8660254037844387076, 1.000000000000000000, 0.8660254037844387076, 1.000000000000000000, 0.8660254037844387076, 1.000000000000000000, 0.8660254037844387076, 1.000000000000000000, 0.8660254037844387076, 1.000000000000000000, 0.8660254037844387076, 1.000000000000000000, 0.8660254037844387076, 1.000000000000000000, 0.8660254037844387076, 1.000000000000000000, 0.8660254037844387076, 1.000000000000000000, 0.8660254037844387076, 1.000000000000000000, 0.8660254037844387076, 1.000000000000000000, 0.8660254037844387076, 1.000000000000000000, 0.8660254037844387076, 1.000000000000000000, 0.8660254037844387076, 1.000000000000000000, 0.8660254037844387076, 1.000000000000000000, 0.8660254037844387076, 1.000000000000000000, 0.9111405360107203144, 0.9401542295229963209),
 ( 1.000000000000000000, 0.8660254037844387076, 1.000000000000000000, 0.8660254037844387076, 1.000000000000000000, 0.8660254037844387076, 1.000000000000000000, 0.8660254037844387076, 1.000000000000000000, 0.8660254037844387076, 1.000000000000000000, 0.8660254037844387076, 1.000000000000000000, 0.8660254037844387076, 1.000000000000000000, 0.8660254037844387076, 1.000000000000000000, 0.8660254037844387076, 1.000000000000000000, 0.8660254037844387076, 1.000000000000000000, 0.8660254037844387076, 1.000000000000000000, 0.8660254037844387076, 1.000000000000000000, 0.8660254037844387076, 1.000000000000000000, 0.8660254037844387076, 1.000000000000000000, 0.8660254037844387076, 1.000000000000000000, 0.8660254037844387076, 1.000000000000000000, 0.8660254037844387076, 1.000000000000000000, 0.8660254037844387076, 1.000000000000000000, 0.8660254037844387076, 1.000000000000000000, 0.8660254037844387076, 1.000000000000000000, 0.8660254037844387076, 1.000000000000000000, 0.8660254037844387076, 1.000000000000000000, 0.8660254037844387076, 1.000000000000000000, 0.8660254037844387076, 1.000000000000000000, 0.8660254037844387076, 1.000000000000000000, 0.8660254037844387076, 1.000000000000000000, 0.8660254037844387076, 1.000000000000000000, 0.8660254037844387076, 1.000000000000000000, 0.8660254037844387076, 1.000000000000000000, 0.8660254037844387076, 1.000000000000000000, 0.8660254037844387076, 1.000000000000000000, 0.8660254037844387076, 1.000000000000000000, 0.8660254037844387076, 1.000000000000000000, 0.8660254037844387076, 1.000000000000000000, 0.8660254037844387076, 1.000000000000000000, 0.8660254037844387076, 1.000000000000000000, 0.8660254037844387076, 1.000000000000000000, 0.8660254037844387076, 1.000000000000000000, 0.8660254037844387076, 1.000000000000000000, 0.8660254037844387076, 1.000000000000000000, 0.8660254037844387076, 1.000000000000000000, 0.8660254037844387076, 1.000000000000000000, 0.8660254037844387076, 1.000000000000000000, 0.8660254037844387076, 1.000000000000000000, 0.8660254037844387076, 1.000000000000000000, 0.8660254037844387076, 1.000000000000000000, 0.8660254037844387076, 1.000000000000000000, 0.8660254037844387076, 1.000000000000000000, 0.8660254037844387076, 1.000000000000000000, 0.8660254037844387076, 1.000000000000000000, 0.8660254037844387076, 1.000000000000000000, 0.8660254037844387076, 1.000000000000000000, 0.8660254037844387076, 1.000000000000000000, 0.8660254037844387076, 1.000000000000000000, 0.8660254037844387076, 1.000000000000000000, 0.8660254037844387076, 1.000000000000000000, 0.8660254037844387076, 1.000000000000000000, 0.8660254037844387076, 1.000000000000000000, 0.8660254037844387076, 1.000000000000000000, 0.8660254037844387076, 1.000000000000000000, 0.8660254037844387076, 1.000000000000000000, 0.8660254037844387076, 1.000000000000000000, 0.8660254037844387076, 1.000000000000000000, 0.8660254037844387076, 1.000000000000000000, 0.8660254037844387076, 1.000000000000000000, 0.8660254037844387076, 1.000000000000000000, 0.9111405360107203144, 0.9401542295229963209) ) ) 
 REPRESENTATION_ITEM ( '' )  SURFACE ( )  );
#9337 = EDGE_CURVE ( 'NONE', #11694, #4350, #5199, .T. ) ;
#9338 = CARTESIAN_POINT ( 'NONE',  ( 82.39999999999999147, -34.61250000000000426, -96.53589838486223584 ) ) ;
#9339 = LINE ( 'NONE', #10807, #7029 ) ;
#9340 = CARTESIAN_POINT ( 'NONE',  ( -83.77821517812500929, -35.12812499938548427, -97.61286128772489690 ) ) ;
#9341 = CARTESIAN_POINT ( 'NONE',  ( 233.4038475772933054, -32.96115380933862582, -47.00000000000010658 ) ) ;
#9342 = CARTESIAN_POINT ( 'NONE',  ( 231.2217848218749339, -34.22812499938548569, 102.3871387122750889 ) ) ;
#9343 = CARTESIAN_POINT ( 'NONE',  ( -83.90000000000000568, -33.62268749875867968, 97.40192378864668399 ) ) ;
#9344 = VERTEX_POINT ( 'NONE', #8226 ) ;
#9345 = CARTESIAN_POINT ( 'NONE',  ( 118.5000000000000284, 12.69999999999998508, 112.0000000000000142 ) ) ;
#9346 = CARTESIAN_POINT ( 'NONE',  ( 5.599999999999999645, 4.041451884327382338, 0.000000000000000000 ) ) ;
#9347 = CARTESIAN_POINT ( 'NONE',  ( 229.8538686580537842, -31.99999999999998579, 99.70214005991812201 ) ) ;
#9348 = CARTESIAN_POINT ( 'NONE',  ( 79.39999999999999147, -34.27499999999999858, 99.99999999999998579 ) ) ;
#9349 = CARTESIAN_POINT ( 'NONE',  ( 85.40000000000000568, -32.73750000000000426, -98.26794919243111792 ) ) ;
#9350 = CARTESIAN_POINT ( 'NONE',  ( 82.39999999999999147, -32.16562499938549280, -96.81714838363319586 ) ) ;
#9351 = DIRECTION ( 'NONE',  ( -0.000000000000000000, -1.000000000000000000, -0.000000000000000000 ) ) ;
#9352 = EDGE_CURVE ( 'NONE', #8610, #3766, #5594, .T. ) ;
#9353 = ORIENTED_EDGE ( 'NONE', *, *, #782, .T. ) ;
#9354 = CARTESIAN_POINT ( 'NONE',  ( 233.9782151781249411, -32.20312499938548001, -52.38713871227520968 ) ) ;
#9355 = B_SPLINE_CURVE_WITH_KNOTS ( 'NONE', 1,
 ( #2058, #4906 ),
 .UNSPECIFIED., .F., .F.,
 ( 2, 2 ),
 ( 0.000000000000000000, 1.000000000000000000 ),
 .UNSPECIFIED. ) ;
#9356 = DIRECTION ( 'NONE',  ( -1.000000000000000000, -1.336382355046098552E-47, 4.814824860968092260E-31 ) ) ;
#9357 = CARTESIAN_POINT ( 'NONE',  ( 229.8435696437499871, -32.01562499938548001, 101.5914258081833879 ) ) ;
#9358 = EDGE_CURVE ( 'NONE', #12231, #927, #8835, .T. ) ;
#9359 = CARTESIAN_POINT ( 'NONE',  ( 235.5999999999999943, -35.15624999877096002, -48.26794919243124582 ) ) ;
#9360 = CARTESIAN_POINT ( 'NONE',  ( -83.77821517812500929, -34.71562499938548285, 97.61286128772489690 ) ) ;
#9361 = ORIENTED_EDGE ( 'NONE', *, *, #10075, .F. ) ;
#9362 = EDGE_LOOP ( 'NONE', ( #19251, #5267, #17151, #59, #617 ) ) ;
#9363 = CARTESIAN_POINT ( 'NONE',  ( -80.60346964444562445, -32.00000000000000000, 97.67482724152021945 ) ) ;
#9364 = LINE ( 'NONE', #15326, #1015 ) ;
#9365 = ORIENTED_EDGE ( 'NONE', *, *, #18905, .T. ) ;
#9366 = DIRECTION ( 'NONE',  ( 0.000000000000000000, 0.000000000000000000, -1.000000000000000000 ) ) ;
#9367 = CARTESIAN_POINT ( 'NONE',  ( -83.90000000000000568, -33.16874999877096286, -102.5980762113533018 ) ) ;
#9368 = CARTESIAN_POINT ( 'NONE',  ( 99.99999999999995737, -21.80000000000003268, -139.9999999999999716 ) ) ;
#9369 = CARTESIAN_POINT ( 'NONE',  ( -85.40000000000000568, -32.64374999877097139, 99.99999999999998579 ) ) ;
#9370 = CARTESIAN_POINT ( 'NONE',  ( -80.90000000000000568, -33.24374999877097281, 97.40192378864668399 ) ) ;
#9371 = CARTESIAN_POINT ( 'NONE',  ( 84.97511176746692740, -34.99999999999998579, -98.48300226792312628 ) ) ;
#9372 = DIRECTION ( 'NONE',  ( -0.000000000000000000, 0.000000000000000000, 1.000000000000000000 ) ) ;
#9373 = FACE_BOUND ( 'NONE', #29, .T. ) ;
#9374 = CARTESIAN_POINT ( 'NONE',  ( 229.8435696437499587, -35.11426541925032296, 98.99674735228809652 ) ) ;
#9375 = CARTESIAN_POINT ( 'NONE',  ( 232.5999999999999375, -31.82812499938547290, 103.1828516163667899 ) ) ;
#9376 = VERTEX_POINT ( 'NONE', #6955 ) ;
#9377 = CARTESIAN_POINT ( 'NONE',  ( 229.5999999999999375, -30.39374999877096428, 99.99999999999998579 ) ) ;
#9378 = LINE ( 'NONE', #15344, #13646 ) ;
#9379 = ORIENTED_EDGE ( 'NONE', *, *, #11272, .T. ) ;
#9380 = DIRECTION ( 'NONE',  ( 0.000000000000000000, 0.000000000000000000, 1.000000000000000000 ) ) ;
#9381 = DIRECTION ( 'NONE',  ( 0.000000000000000000, 0.000000000000000000, -1.000000000000000000 ) ) ;
#9382 = UNCERTAINTY_MEASURE_WITH_UNIT (LENGTH_MEASURE( 1.000000000000000082E-05 ), #7132, 'distance_accuracy_value', 'NONE');
#9383 = CARTESIAN_POINT ( 'NONE',  ( 81.59615242270662350, -33.46740381056766722, 96.99999999999998579 ) ) ;
#9384 = ORIENTED_EDGE ( 'NONE', *, *, #3608, .T. ) ;
#9385 = CARTESIAN_POINT ( 'NONE',  ( 229.5999999999999375, -33.50624999877096144, 101.7320508075688821 ) ) ;
#9386 = ORIENTED_EDGE ( 'NONE', *, *, #3943, .F. ) ;
#9387 = VERTEX_POINT ( 'NONE', #5497 ) ;
#9388 =( BOUNDED_CURVE ( )  B_SPLINE_CURVE ( 2, ( #18026, #4733, #10679, #3249, #14685, #1320, #2157, #350, #1789 ),
 .UNSPECIFIED., .F., .F. ) 
 B_SPLINE_CURVE_WITH_KNOTS ( ( 3, 2, 2, 2, 3 ),
 ( 0.7291666666666668517, 0.7361111111111111605, 0.7500000000000000000, 0.7638888888888888395, 0.7708333333333332593 ),
 .UNSPECIFIED. ) 
 CURVE ( )  GEOMETRIC_REPRESENTATION_ITEM ( )  RATIONAL_B_SPLINE_CURVE ( ( 0.9330127018922194093, 0.9330127018922209636, 1.000000000000000000, 0.8660254037844387076, 1.000000000000000000, 0.8660254037844387076, 1.000000000000000000, 0.9330127018922198534, 0.9330127018922192983 ) ) 
 REPRESENTATION_ITEM ( '' )  );
#9389 = CARTESIAN_POINT ( 'NONE',  ( -81.01744233620662783, -32.00000000000001421, 102.5835086888313015 ) ) ;
#9390 = CARTESIAN_POINT ( 'NONE',  ( 83.90000000000000568, -30.37500000000000355, -102.5980762113533018 ) ) ;
#9391 = CARTESIAN_POINT ( 'NONE',  ( -4.000000000000000000, -0.3979232138631226823, -3.896351557369779711E-17 ) ) ;
#9392 = CARTESIAN_POINT ( 'NONE',  ( -85.40000000000000568, -35.30624999877096570, 101.7320508075688679 ) ) ;
#9393 = EDGE_CURVE ( 'NONE', #5172, #9425, #8278, .T. ) ;
#9394 = PRODUCT_RELATED_PRODUCT_CATEGORY ( 'part', '', ( #18891 ) ) ;
#9395 = CARTESIAN_POINT ( 'NONE',  ( -80.90000000000000568, -33.39374999877097139, 102.5980762113533018 ) ) ;
#9396 = CARTESIAN_POINT ( 'NONE',  ( 79.39999999999999147, -33.31874999877096855, 99.99999999999998579 ) ) ;
#9397 =( BOUNDED_CURVE ( )  B_SPLINE_CURVE ( 2, ( #8576, #3996, #11422, #883, #11607, #5377, #14341, #18949, #2431 ),
 .UNSPECIFIED., .F., .F. ) 
 B_SPLINE_CURVE_WITH_KNOTS ( ( 3, 2, 2, 2, 3 ),
 ( 0.7708333333333331483, 0.7777777777777777901, 0.7916666666666666297, 0.8055555555555555802, 0.8125000000000001110 ),
 .UNSPECIFIED. ) 
 CURVE ( )  GEOMETRIC_REPRESENTATION_ITEM ( )  RATIONAL_B_SPLINE_CURVE ( ( 0.9330127018922194093, 0.9330127018922177440, 1.000000000000000000, 0.8660254037844387076, 1.000000000000000000, 0.8660254037844387076, 1.000000000000000000, 0.9330127018922182991, 0.9330127018922194093 ) ) 
 REPRESENTATION_ITEM ( '' )  );
#9398 = CARTESIAN_POINT ( 'NONE',  ( 82.39999999999999147, -33.51562499938548711, -96.81714838363319586 ) ) ;
#9399 = DIRECTION ( 'NONE',  ( 0.000000000000000000, 0.000000000000000000, -1.000000000000000000 ) ) ;
#9400 = MANIFOLD_SOLID_BREP ( 'M5 Clearance Hole1', #17271 ) ;
#9401 = CARTESIAN_POINT ( 'NONE',  ( -85.15643035624999868, -33.32812499938548001, 98.40857419181659793 ) ) ;
#9402 = CARTESIAN_POINT ( 'NONE',  ( 81.02178482187500208, -34.79062499938548569, -97.61286128772489690 ) ) ;
#9403 = ORIENTED_EDGE ( 'NONE', *, *, #14251, .F. ) ;
#9404 = CARTESIAN_POINT ( 'NONE',  ( 234.0999999999999375, -32.09999999999999432, -47.40192378864679768 ) ) ;
#9405 = CARTESIAN_POINT ( 'NONE',  ( 232.5999999999999091, -34.38749999999999574, 102.9999999999999858 ) ) ;
#9406 = CARTESIAN_POINT ( 'NONE',  ( 83.90000000000000568, -33.61874999877097281, -97.40192378864668399 ) ) ;
#9407 = CARTESIAN_POINT ( 'NONE',  ( 85.40000000000000568, -33.56250000000000000, 98.26794919243111792 ) ) ;
#9408 = CARTESIAN_POINT ( 'NONE',  ( -82.39999999999999147, -32.61562499938548854, 96.81714838363319586 ) ) ;
#9409 = CARTESIAN_POINT ( 'NONE',  ( 233.9782151781249411, -32.65312499938548285, -52.38713871227520968 ) ) ;
#9410 = CARTESIAN_POINT ( 'NONE',  ( -80.90000000000000568, -32.10000000000000142, 102.5980762113533018 ) ) ;
#9411 = ORIENTED_EDGE ( 'NONE', *, *, #11727, .T. ) ;
#9412 = CARTESIAN_POINT ( 'NONE',  ( -85.10336890117802966, -34.99999999999999289, 100.9939266215828724 ) ) ;
#9413 = CARTESIAN_POINT ( 'NONE',  ( -79.39999999999999147, -34.66874999877096997, 99.99999999999998579 ) ) ;
#9414 = CARTESIAN_POINT ( 'NONE',  ( 82.39999999999999147, -32.72812499938548569, 96.81714838363319586 ) ) ;
#9415 = AXIS2_PLACEMENT_3D ( 'NONE', #710, #3910, #14169 ) ;
#9416 = CARTESIAN_POINT ( 'NONE',  ( 234.0999999999999375, -34.79999999999999716, 102.5980762113533018 ) ) ;
#9417 =( BOUNDED_CURVE ( )  B_SPLINE_CURVE ( 2, ( #15207, #377, #17263, #2401, #17549 ),
 .UNSPECIFIED., .F., .F. ) 
 B_SPLINE_CURVE_WITH_KNOTS ( ( 3, 2, 3 ),
 ( 0.2975293541897461869, 0.3055555555555555802, 0.3125000000000001665 ),
 .UNSPECIFIED. ) 
 CURVE ( )  GEOMETRIC_REPRESENTATION_ITEM ( )  RATIONAL_B_SPLINE_CURVE ( ( 0.9346381638529985825, 0.9225778897267049583, 1.000000000000000000, 0.9330127018922177440, 0.9330127018922194093 ) ) 
 REPRESENTATION_ITEM ( '' )  );
#9418 = CARTESIAN_POINT ( 'NONE',  ( -85.15643035625001289, -32.09062499938548996, 98.40857419181659793 ) ) ;
#9419 = CARTESIAN_POINT ( 'NONE',  ( 80.42036527867306006, -31.99999999999999289, 97.80162405160976391 ) ) ;
#9420 = CARTESIAN_POINT ( 'NONE',  ( 79.64356964375001269, -35.01562499938548711, 98.40857419181659793 ) ) ;
#9421 = CARTESIAN_POINT ( 'NONE',  ( 82.39999999999999147, -31.49062499938548854, -103.1828516163667899 ) ) ;
#9422 = CARTESIAN_POINT ( 'NONE',  ( 233.4038475772933054, -33.01740381056766438, -47.00000000000009237 ) ) ;
#9423 = CARTESIAN_POINT ( 'NONE',  ( -79.64356964374999848, -34.07812499938548711, 99.99999999999998579 ) ) ;
#9424 = CARTESIAN_POINT ( 'NONE',  ( -82.39999999999999147, -33.29062499938549280, -96.81714838363319586 ) ) ;
#9425 = VERTEX_POINT ( 'NONE', #9785 ) ;
#9426 = CARTESIAN_POINT ( 'NONE',  ( 85.15643035625001289, -33.85312499938549280, 99.99999999999998579 ) ) ;
#9427 = EDGE_CURVE ( 'NONE', #19103, #3788, #12712, .T. ) ;
#9428 = DIRECTION ( 'NONE',  ( 0.000000000000000000, -1.000000000000000000, 0.000000000000000000 ) ) ;
#9429 = AXIS2_PLACEMENT_3D ( 'NONE', #10459, #1388, #10365 ) ;
#9430 = CARTESIAN_POINT ( 'NONE',  ( -81.02178482187500208, -30.29062499938548569, 97.61286128772489690 ) ) ;
#9431 = CIRCLE ( 'NONE', #18178, 5.000000000000000000 ) ;
#9432 = CARTESIAN_POINT ( 'NONE',  ( -79.64356964375001269, -34.04062499938549280, 98.40857419181659793 ) ) ;
#9433 = CARTESIAN_POINT ( 'NONE',  ( 235.4117376914898898, -32.00000000000000000, -51.04600724388262023 ) ) ;
#9434 = ORIENTED_EDGE ( 'NONE', *, *, #5054, .F. ) ;
#9435 = CARTESIAN_POINT ( 'NONE',  ( -85.40000000000000568, -34.53750000000000142, -101.7320508075688679 ) ) ;
#9436 = CARTESIAN_POINT ( 'NONE',  ( -80.90000000000000568, -32.34374999877096712, 97.40192378864668399 ) ) ;
#9437 = CARTESIAN_POINT ( 'NONE',  ( -82.40000000000000568, -30.00000000000000355, 96.99999999999998579 ) ) ;
#9438 = CARTESIAN_POINT ( 'NONE',  ( -79.64356964374999848, -34.97812499938548569, -99.99999999999998579 ) ) ;
#9439 = CARTESIAN_POINT ( 'NONE',  ( 235.3564303562499447, -33.17812499938548143, 99.99999999999998579 ) ) ;
#9440 = CARTESIAN_POINT ( 'NONE',  ( -85.40000000000000568, -33.13518749875868252, 98.26794919243111792 ) ) ;
#9441 = ORIENTED_EDGE ( 'NONE', *, *, #18735, .F. ) ;
#9442 = CYLINDRICAL_SURFACE ( 'NONE', #15552, 3.000000000000002665 ) ;
#9443 = DIRECTION ( 'NONE',  ( -1.000000000000000000, 4.625929269271494788E-16, 0.000000000000000000 ) ) ;
#9444 = CARTESIAN_POINT ( 'NONE',  ( -82.40000000000000568, -33.03750000000000142, 102.9999999999999858 ) ) ;
#9445 = CARTESIAN_POINT ( 'NONE',  ( 79.39999999999999147, -34.23750000000000426, 101.7320508075688963 ) ) ;
#9446 = CIRCLE ( 'NONE', #13198, 2.649999999999982148 ) ;
#9447 = CARTESIAN_POINT ( 'NONE',  ( -82.39999999999999147, -34.33124999877097139, 103.0000000000000000 ) ) ;
#9448 = CARTESIAN_POINT ( 'NONE',  ( 79.64356964375001269, -30.96562499938548640, -101.5914258081833879 ) ) ;
#9449 = CARTESIAN_POINT ( 'NONE',  ( 4.082498951862916670, 2.020725942163688504, 3.500000000000000000 ) ) ;
#9450 = ORIENTED_EDGE ( 'NONE', *, *, #4839, .T. ) ;
#9451 = FACE_OUTER_BOUND ( 'NONE', #6062, .T. ) ;
#9452 = APPLICATION_PROTOCOL_DEFINITION ( 'draft international standard', 'automotive_design', 1998, #3323 ) ;
#9453 = CARTESIAN_POINT ( 'NONE',  ( 235.3564303562499447, -31.79062499938547859, 98.40857419181659793 ) ) ;
#9454 = CARTESIAN_POINT ( 'NONE',  ( 229.5999999999999375, -35.30624999877095860, -48.26794919243123161 ) ) ;
#9455 =( BOUNDED_CURVE ( )  B_SPLINE_CURVE ( 2, ( #17294, #1168, #8394, #7216, #15826, #7127, #14439, #10255, #16216 ),
 .UNSPECIFIED., .F., .F. ) 
 B_SPLINE_CURVE_WITH_KNOTS ( ( 3, 2, 2, 2, 3 ),
 ( 0.6875000000000000000, 0.6944444444444444198, 0.7083333333333333703, 0.7222222222222222099, 0.7291666666666666297 ),
 .UNSPECIFIED. ) 
 CURVE ( )  GEOMETRIC_REPRESENTATION_ITEM ( )  RATIONAL_B_SPLINE_CURVE ( ( 0.9330127018922194093, 0.9330127018922194093, 1.000000000000000000, 0.8660254037844387076, 1.000000000000000000, 0.8660254037844387076, 1.000000000000000000, 0.9330127018922198534, 0.9330127018922192983 ) ) 
 REPRESENTATION_ITEM ( '' )  );
#9456 = CARTESIAN_POINT ( 'NONE',  ( -79.64356964375001269, -32.57812499938548001, 98.40857419181659793 ) ) ;
#9457 = CARTESIAN_POINT ( 'NONE',  ( 233.4038475772933339, -34.63259618943233420, -53.00000000000009948 ) ) ;
#9458 = ORIENTED_EDGE ( 'NONE', *, *, #3170, .F. ) ;
#9459 = ORIENTED_EDGE ( 'NONE', *, *, #7442, .F. ) ;
#9460 = CARTESIAN_POINT ( 'NONE',  ( 4.151274195509476073, 2.039912954708820170, -3.533232880573633050 ) ) ;
#9461 = DIRECTION ( 'NONE',  ( -0.000000000000000000, -1.000000000000000000, -0.000000000000000000 ) ) ;
#9462 = DIRECTION ( 'NONE',  ( 1.000000000000000000, 0.000000000000000000, 0.000000000000000000 ) ) ;
#9463 = ORIENTED_EDGE ( 'NONE', *, *, #4373, .F. ) ;
#9464 = DIRECTION ( 'NONE',  ( -0.000000000000000000, -0.000000000000000000, 1.000000000000000000 ) ) ;
#9465 = CARTESIAN_POINT ( 'NONE',  ( -82.39999999999999147, -34.78124999877096712, -96.53589838486223584 ) ) ;
#9466 = B_SPLINE_CURVE_WITH_KNOTS ( 'NONE', 3,
 ( #12334, #722, #6478, #10865, #5019, #16929, #3540, #9495 ),
 .UNSPECIFIED., .F., .F.,
 ( 4, 2, 2, 4 ),
 ( 2.465131517071352357E-07, 0.001183067374689843057, 0.001774477805458910071, 0.002365888236227977302 ),
 .UNSPECIFIED. ) ;
#9467 = MANIFOLD_SOLID_BREP ( 'Thread1', #3526 ) ;
#9468 = EDGE_CURVE ( 'NONE', #5107, #5933, #15297, .T. ) ;
#9469 = CARTESIAN_POINT ( 'NONE',  ( -79.39999999999999147, -32.06250000000000000, 101.7320508075688537 ) ) ;
#9470 = CARTESIAN_POINT ( 'NONE',  ( -82.39999999999999147, -32.08124999877097139, 103.4641016151377499 ) ) ;
#9471 = CARTESIAN_POINT ( 'NONE',  ( -82.39999999999999147, -34.55624999877096570, 96.53589838486223584 ) ) ;
#9472 = DIRECTION ( 'NONE',  ( 1.224646799147353207E-16, 1.000000000000000000, 0.000000000000000000 ) ) ;
#9473 = CARTESIAN_POINT ( 'NONE',  ( 232.5999999999999375, -33.88124999877096855, -47.00000000000011369 ) ) ;
#9474 = CARTESIAN_POINT ( 'NONE',  ( 233.4038475772933339, -33.46740381056766012, 102.9999999999999716 ) ) ;
#9475 = CARTESIAN_POINT ( 'NONE',  ( 229.8435696437499303, -34.64062499938548001, 99.99999999999998579 ) ) ;
#9476 = EDGE_CURVE ( 'NONE', #4279, #11737, #12464, .T. ) ;
#9477 = ORIENTED_EDGE ( 'NONE', *, *, #4995, .F. ) ;
#9478 = CARTESIAN_POINT ( 'NONE',  ( -85.15643035624999868, -35.11426555956768425, -101.0032586025029815 ) ) ;
#9479 = CARTESIAN_POINT ( 'NONE',  ( 4.114405500665261783, 4.051151509359415925, -1.111238067874716415E-16 ) ) ;
#9480 = ORIENTED_EDGE ( 'NONE', *, *, #2039, .F. ) ;
#9481 = CARTESIAN_POINT ( 'NONE',  ( -80.90000000000000568, -33.45000000000000284, -97.40192378864668399 ) ) ;
#9482 = DIRECTION ( 'NONE',  ( 1.788378118793198438E-31, 3.597944987211154374E-15, 1.000000000000000000 ) ) ;
#9483 = CARTESIAN_POINT ( 'NONE',  ( 80.90000000000000568, -32.10000000000000142, 97.40192378864668399 ) ) ;
#9484 = ORIENTED_EDGE ( 'NONE', *, *, #19165, .T. ) ;
#9485 = CARTESIAN_POINT ( 'NONE',  ( 232.5999999999999375, -34.97812499938547859, -46.81714838363331666 ) ) ;
#9486 = ORIENTED_EDGE ( 'NONE', *, *, #13776, .T. ) ;
#9487 = ORIENTED_EDGE ( 'NONE', *, *, #6998, .F. ) ;
#9488 = CARTESIAN_POINT ( 'NONE',  ( 109.9999999999999574, -21.80000000000003268, -142.6499999999999773 ) ) ;
#9489 = CARTESIAN_POINT ( 'NONE',  ( 84.51155491706698797, -35.14114833091483803, -98.22820877610629964 ) ) ;
#9490 = CARTESIAN_POINT ( 'NONE',  ( -82.40000000000000568, -30.00000000000000355, -99.99999999999998579 ) ) ;
#9491 = EDGE_CURVE ( 'NONE', #9205, #8694, #7328, .T. ) ;
#9492 = CARTESIAN_POINT ( 'NONE',  ( -85.40000000000000568, -33.95624999877097139, 101.7320508075688679 ) ) ;
#9493 = CARTESIAN_POINT ( 'NONE',  ( -85.40000000000000568, -34.08356250001229171, 98.26794919243111792 ) ) ;
#9494 = CARTESIAN_POINT ( 'NONE',  ( -79.39999999999999147, -33.35624999877096997, 101.7320508075688537 ) ) ;
#9495 = CARTESIAN_POINT ( 'NONE',  ( -2.000000000000006661, 3.464101615137750834, 0.000000000000000000 ) ) ;
#9496 = EDGE_CURVE ( 'NONE', #16323, #12516, #18831, .T. ) ;
#9497 = CARTESIAN_POINT ( 'NONE',  ( 81.02178482187500208, -34.15312499938548285, -102.3871387122750889 ) ) ;
#9498 = CARTESIAN_POINT ( 'NONE',  ( 3.951447005078451813, -1.347150628109132553, -3.500000000000000444 ) ) ;
#9499 = CARTESIAN_POINT ( 'NONE',  ( -85.15643035624999868, -32.35312499938549280, 101.5914258081833879 ) ) ;
#9500 = CARTESIAN_POINT ( 'NONE',  ( 79.64356964374999848, -34.41562499938548569, -99.99999999999998579 ) ) ;
#9501 = ORIENTED_EDGE ( 'NONE', *, *, #15830, .T. ) ;
#9502 = CARTESIAN_POINT ( 'NONE',  ( 235.5999999999999375, -32.02499999999999858, -50.00000000000011369 ) ) ;
#9503 = CARTESIAN_POINT ( 'NONE',  ( -79.39999999999999147, -33.78750000000000142, 98.26794919243110371 ) ) ;
#9504 = PRODUCT_DEFINITION_SHAPE ( 'NONE', 'NONE',  #19334 ) ;
#9505 = CARTESIAN_POINT ( 'NONE',  ( 118.5000000000000284, 12.69999999999998508, 30.20101012677667285 ) ) ;
#9506 = CARTESIAN_POINT ( 'NONE',  ( 231.2217848218749339, -33.47812499938547859, 97.61286128772489690 ) ) ;
#9507 = CARTESIAN_POINT ( 'NONE',  ( -79.64356964375001269, -31.34062499938548640, 98.40857419181659793 ) ) ;
#9508 = ADVANCED_FACE ( 'NONE', ( #17986 ), #14650, .T. ) ;
#9509 = CARTESIAN_POINT ( 'NONE',  ( 229.8435696437499303, -33.85312499938548569, -50.00000000000011369 ) ) ;
#9510 = CARTESIAN_POINT ( 'NONE',  ( -82.39999999999999147, -32.58750000000000568, 103.4641016151377499 ) ) ;
#9511 = ORIENTED_EDGE ( 'NONE', *, *, #16891, .T. ) ;
#9512 = CARTESIAN_POINT ( 'NONE',  ( -94.79999999999999716, -32.00000000000000000, -150.0000000000000000 ) ) ;
#9513 =( BOUNDED_CURVE ( )  B_SPLINE_CURVE ( 2, ( #8083, #9649, #6240, #4778, #3290, #15215, #18253, #1831, #6336 ),
 .UNSPECIFIED., .F., .F. ) 
 B_SPLINE_CURVE_WITH_KNOTS ( ( 3, 2, 2, 2, 3 ),
 ( 0.3958333333333334259, 0.4027777777777777901, 0.4166666666666666852, 0.4305555555555555802, 0.4375000000000000555 ),
 .UNSPECIFIED. ) 
 CURVE ( )  GEOMETRIC_REPRESENTATION_ITEM ( )  RATIONAL_B_SPLINE_CURVE ( ( 0.9330127018922192983, 0.9330127018922200755, 1.000000000000000000, 0.8660254037844387076, 1.000000000000000000, 0.8660254037844387076, 1.000000000000000000, 0.9330127018922187432, 0.9330127018922192983 ) ) 
 REPRESENTATION_ITEM ( '' )  );
#9514 = CARTESIAN_POINT ( 'NONE',  ( 4.050536630291690976, 3.778525289263159781, 0.5912575323401411120 ) ) ;
#9515 = CARTESIAN_POINT ( 'NONE',  ( 83.77821517812500929, -32.31562499938548427, 97.61286128772489690 ) ) ;
#9516 = VECTOR ( 'NONE', #9464, 1000.000000000000000 ) ;
#9517 = CARTESIAN_POINT ( 'NONE',  ( 233.4038475772933339, -34.81740381056766154, 102.9999999999999716 ) ) ;
#9518 = ADVANCED_FACE ( 'NONE', ( #2634 ), #19256, .F. ) ;
#9519 = CARTESIAN_POINT ( 'NONE',  ( -83.77821517812500929, -32.12812499938548427, 97.61286128772489690 ) ) ;
#9520 = CARTESIAN_POINT ( 'NONE',  ( -79.64356964374998427, -32.69062499938548427, -101.5914258081833879 ) ) ;
#9521 = CARTESIAN_POINT ( 'NONE',  ( 82.39999999999999147, -30.47812499938548569, 96.81714838363319586 ) ) ;
#9522 = CARTESIAN_POINT ( 'NONE',  ( 85.15643035625001289, -31.15312499938548996, -99.99999999999998579 ) ) ;
#9523 = CARTESIAN_POINT ( 'NONE',  ( 231.2217848218749339, -30.21562499938547575, -52.38713871227520968 ) ) ;
#9524 = CARTESIAN_POINT ( 'NONE',  ( -79.64356964374998427, -33.21562499938548996, 101.5914258081833879 ) ) ;
#9525 = CARTESIAN_POINT ( 'NONE',  ( -85.15643035624999868, -33.36562499938548854, -98.40857419181659793 ) ) ;
#9526 = ORIENTED_EDGE ( 'NONE', *, *, #2437, .T. ) ;
#9527 = CARTESIAN_POINT ( 'NONE',  ( 81.02178482187500208, -32.65312499938548996, 102.3871387122750889 ) ) ;
#9528 = CARTESIAN_POINT ( 'NONE',  ( 3.974175853610028231, -2.726149789692840386, -2.409821656223227748 ) ) ;
#9529 = CIRCLE ( 'NONE', #12029, 5.199999999999996625 ) ;
#9530 = CARTESIAN_POINT ( 'NONE',  ( -85.15643035625001289, -31.49062499938548498, 99.99999999999998579 ) ) ;
#9531 = CARTESIAN_POINT ( 'NONE',  ( -82.39999999999999147, -33.06562499938548427, 96.81714838363319586 ) ) ;
#9532 = CARTESIAN_POINT ( 'NONE',  ( -1.312671235360383548, -3.860931062424228788, -0.05923475698271369466 ) ) ;
#9533 = EDGE_LOOP ( 'NONE', ( #16683, #13175, #14475, #972, #9819 ) ) ;
#9534 = CARTESIAN_POINT ( 'NONE',  ( -79.39999999999999147, -33.86250000000000426, -98.26794919243113213 ) ) ;
#9535 = DIRECTION ( 'NONE',  ( -0.000000000000000000, -1.000000000000000000, -0.000000000000000000 ) ) ;
#9536 = DIRECTION ( 'NONE',  ( 0.000000000000000000, 0.000000000000000000, -1.000000000000000000 ) ) ;
#9537 = CARTESIAN_POINT ( 'NONE',  ( -83.77821517812500929, -34.67812499938548854, -97.61286128772489690 ) ) ;
#9538 = CARTESIAN_POINT ( 'NONE',  ( 235.3564303562499447, -33.21562499938548285, 101.5914258081833879 ) ) ;
#9539 = CARTESIAN_POINT ( 'NONE',  ( -85.40000000000000568, -34.48518749875868394, 98.26794919243111792 ) ) ;
#9540 = ORIENTED_EDGE ( 'NONE', *, *, #10001, .T. ) ;
#9541 = CARTESIAN_POINT ( 'NONE',  ( -82.39999999999999147, -35.09062499938548285, 103.1828516163667899 ) ) ;
#9542 = CARTESIAN_POINT ( 'NONE',  ( -82.40000000000000568, -35.00000000000000000, 99.99999999999998579 ) ) ;
#9543 = CARTESIAN_POINT ( 'NONE',  ( -85.27821517812500929, -30.07031249969274356, 99.99999999999998579 ) ) ;
#9544 = CARTESIAN_POINT ( 'NONE',  ( 94.79999999999995453, -32.00000000000000000, -150.0000000000000000 ) ) ;
#9545 = VECTOR ( 'NONE', #15285, 1000.000000000000000 ) ;
#9546 = CARTESIAN_POINT ( 'NONE',  ( 110.0000000000000568, 5.199999999999975309, -147.9289321881345245 ) ) ;
#9547 = CARTESIAN_POINT ( 'NONE',  ( 79.64356964375001269, -31.34062499938548640, -98.40857419181659793 ) ) ;
#9548 = DIRECTION ( 'NONE',  ( 0.000000000000000000, -1.000000000000000000, 0.000000000000000000 ) ) ;
#9549 = ORIENTED_EDGE ( 'NONE', *, *, #1020, .T. ) ;
#9550 = CARTESIAN_POINT ( 'NONE',  ( 82.39999999999999147, -31.18124999877096926, 96.53589838486223584 ) ) ;
#9551 = SHAPE_DEFINITION_REPRESENTATION ( #17162, #7749 ) ;
#9552 = CARTESIAN_POINT ( 'NONE',  ( 235.3564303562499447, -32.31562499938547717, 101.5914258081833879 ) ) ;
#9553 = CARTESIAN_POINT ( 'NONE',  ( 235.3564303562499447, -31.86562499938547788, -48.40857419181671162 ) ) ;
#9554 = COLOUR_RGB ( '',1.000000000000000000, 0.9490196078431372140, 0.9098039215686274384 ) ;
#9555 = CARTESIAN_POINT ( 'NONE',  ( -79.64356964374999848, -34.41562499938548569, 99.99999999999998579 ) ) ;
#9556 = CARTESIAN_POINT ( 'NONE',  ( -83.90000000000000568, -34.87500000000000000, 102.5980762113533018 ) ) ;
#9557 = ORIENTED_EDGE ( 'NONE', *, *, #6752, .T. ) ;
#9558 = ORIENTED_EDGE ( 'NONE', *, *, #178, .T. ) ;
#9559 = CARTESIAN_POINT ( 'NONE',  ( -79.64356964375001269, -30.77812499938548285, -101.5914258081833879 ) ) ;
#9560 = CIRCLE ( 'NONE', #12055, 5.199999999999996625 ) ;
#9561 = CARTESIAN_POINT ( 'NONE',  ( 83.20384757729335945, -33.05759618943233136, 96.99999999999998579 ) ) ;
#9562 = VERTEX_POINT ( 'NONE', #14549 ) ;
#9563 = CARTESIAN_POINT ( 'NONE',  ( 79.64356964374998427, -34.56562499938548427, 98.40857419181659793 ) ) ;
#9564 = CARTESIAN_POINT ( 'NONE',  ( -85.40000000000000568, -33.54374999877096286, -99.99999999999998579 ) ) ;
#9565 = CARTESIAN_POINT ( 'NONE',  ( 2.500000000000000888, 3.061616997868384127E-16, -4.974599999999998801 ) ) ;
#9566 = CARTESIAN_POINT ( 'NONE',  ( -83.90000000000000568, -33.16874999877096286, 97.40192378864668399 ) ) ;
#9567 = CARTESIAN_POINT ( 'NONE',  ( -83.90000000000000568, -33.16874999877096286, 97.40192378864668399 ) ) ;
#9568 = CARTESIAN_POINT ( 'NONE',  ( -83.20384757729337366, -32.34240381056766722, 97.00000000000000000 ) ) ;
#9569 = EDGE_LOOP ( 'NONE', ( #13477, #16342 ) ) ;
#9570 = CARTESIAN_POINT ( 'NONE',  ( 232.3466685930879123, -34.99995246259152282, 97.01071553687879145 ) ) ;
#9571 = CARTESIAN_POINT ( 'NONE',  ( -80.90000000000000568, -34.29374999877096997, 102.5980762113533018 ) ) ;
#9572 = AXIS2_PLACEMENT_3D ( 'NONE', #3686, #15412, #17173 ) ;
#9573 = CARTESIAN_POINT ( 'NONE',  ( 235.3564303562499447, -33.47812499938547148, 98.40857419181659793 ) ) ;
#9574 = ORIENTED_EDGE ( 'NONE', *, *, #17389, .F. ) ;
#9575 = CARTESIAN_POINT ( 'NONE',  ( 85.15643035625001289, -33.32812499938548711, -98.40857419181659793 ) ) ;
#9576 = SURFACE_STYLE_USAGE ( .BOTH. , #8214 ) ;
#9577 = CARTESIAN_POINT ( 'NONE',  ( -82.39999999999999147, -34.52812499938548996, -96.81714838363319586 ) ) ;
#9578 = CARTESIAN_POINT ( 'NONE',  ( 231.7961524227065695, -32.10134618820329422, 102.9999999999999716 ) ) ;
#9579 = EDGE_LOOP ( 'NONE', ( #9501, #18079, #12400, #4231, #11243, #12578 ) ) ;
#9580 = DIRECTION ( 'NONE',  ( 1.387778780781445676E-15, 1.000000000000000000, 0.000000000000000000 ) ) ;
#9581 = LINE ( 'NONE', #18478, #7727 ) ;
#9582 = MECHANICAL_DESIGN_GEOMETRIC_PRESENTATION_REPRESENTATION (  '', ( #17704 ), #3343 ) ;
#9583 = CARTESIAN_POINT ( 'NONE',  ( 2.345747346278113987, -3.264484291692503870, -0.01223254789874484924 ) ) ;
#9584 = ORIENTED_EDGE ( 'NONE', *, *, #9167, .T. ) ;
#9585 = CARTESIAN_POINT ( 'NONE',  ( -80.90000000000000568, -31.89374999877096784, 97.40192378864668399 ) ) ;
#9586 = EDGE_CURVE ( 'NONE', #11098, #10346, #7432, .T. ) ;
#9587 = CARTESIAN_POINT ( 'NONE',  ( 4.000000000000003553, -2.309401076758513138, -3.504271511727127031 ) ) ;
#9588 = VERTEX_POINT ( 'NONE', #10271 ) ;
#9589 = CARTESIAN_POINT ( 'NONE',  ( 79.39999999999999147, -33.31874999877096855, -99.99999999999998579 ) ) ;
#9590 = CARTESIAN_POINT ( 'NONE',  ( 85.40000000000000568, -30.00000000000000355, -99.99999999999998579 ) ) ;
#9591 = CARTESIAN_POINT ( 'NONE',  ( 3.973514160553464514, -3.435084588004195805, 1.181876024140317227 ) ) ;
#9592 = VECTOR ( 'NONE', #13351, 1000.000000000000000 ) ;
#9593 = EDGE_CURVE ( 'NONE', #484, #17889, #16232, .T. ) ;
#9594 = CARTESIAN_POINT ( 'NONE',  ( -85.40000000000000568, -34.93124999877096570, 98.26794919243111792 ) ) ;
#9595 = CARTESIAN_POINT ( 'NONE',  ( -84.69814161231455785, -34.99658579608068720, 98.07164704222793716 ) ) ;
#9596 = DIRECTION ( 'NONE',  ( 0.000000000000000000, 0.000000000000000000, -1.000000000000000000 ) ) ;
#9597 = CARTESIAN_POINT ( 'NONE',  ( 82.40000000000000568, -30.00000000000000355, 103.0000000000000000 ) ) ;
#9598 = CARTESIAN_POINT ( 'NONE',  ( 85.15643035625001289, -32.46562499938548996, -101.5914258081833879 ) ) ;
#9599 = VECTOR ( 'NONE', #13586, 1000.000000000000000 ) ;
#9600 = CARTESIAN_POINT ( 'NONE',  ( -79.39999999999999147, -33.76874999877097139, 99.99999999999998579 ) ) ;
#9601 = CARTESIAN_POINT ( 'NONE',  ( -85.15643035624999868, -34.22812499938547859, 98.40857419181659793 ) ) ;
#9602 = CARTESIAN_POINT ( 'NONE',  ( 79.64356964374999848, -32.61562499938548854, -99.99999999999998579 ) ) ;
#9603 = EDGE_LOOP ( 'NONE', ( #13879, #597, #10759, #10616 ) ) ;
#9604 = CARTESIAN_POINT ( 'NONE',  ( 234.9136945297046282, -32.02340763552835057, -47.87171054440991469 ) ) ;
#9605 = CARTESIAN_POINT ( 'NONE',  ( -85.40000000000000568, -33.56250000000000000, 101.7320508075688679 ) ) ;
#9606 = VECTOR ( 'NONE', #11642, 1000.000000000000000 ) ;
#9607 = EDGE_CURVE ( 'NONE', #17054, #16462, #2225, .T. ) ;
#9608 = CARTESIAN_POINT ( 'NONE',  ( 0.1404048886732821022, 4.699864953788070565, -3.686887068327037387 ) ) ;
#9609 = CARTESIAN_POINT ( 'NONE',  ( 83.20384757729337366, -33.50759618943233420, 97.00000000000000000 ) ) ;
#9610 = CARTESIAN_POINT ( 'NONE',  ( -81.02178482187500208, -30.55312499938548854, 102.3871387122750889 ) ) ;
#9611 = EDGE_CURVE ( 'NONE', #13408, #5861, #3025, .T. ) ;
#9612 = CARTESIAN_POINT ( 'NONE',  ( 229.8435696437499871, -32.46562499938548285, -48.40857419181671162 ) ) ;
#9613 = EDGE_CURVE ( 'NONE', #14621, #729, #13478, .T. ) ;
#9614 = CARTESIAN_POINT ( 'NONE',  ( -83.90000000000000568, -32.77499999999999858, 97.40192378864668399 ) ) ;
#9615 = B_SPLINE_CURVE_WITH_KNOTS ( 'NONE', 3,
 ( #18042, #16569, #14606, #1237, #7189, #13138, #2794, #19112, #19314, #5925, #7379, #13237, #11871, #11681, #5732, #17838, #8747, #14699 ),
 .UNSPECIFIED., .F., .F.,
 ( 4, 2, 2, 2, 2, 2, 2, 2, 4 ),
 ( 0.000000000000000000, 0.0007106627595359796094, 0.001421325519071959219, 0.002131988278607938828, 0.002842651038143918438, 0.003553313797679898047, 0.004263976557215877657, 0.004974639316751856832, 0.005685302076287836875 ),
 .UNSPECIFIED. ) ;
#9616 = ORIENTED_EDGE ( 'NONE', *, *, #9613, .T. ) ;
#9617 = DIRECTION ( 'NONE',  ( 1.000000000000000000, 0.000000000000000000, 0.000000000000000000 ) ) ;
#9618 = AXIS2_PLACEMENT_3D ( 'NONE', #4767, #14025, #15298 ) ;
#9619 = CARTESIAN_POINT ( 'NONE',  ( 83.20395887649176814, -35.00000000000001421, 97.36341917746361219 ) ) ;
#9620 = CARTESIAN_POINT ( 'NONE',  ( 79.64356964374999848, -33.51562499938548711, 99.99999999999998579 ) ) ;
#9621 = AXIS2_PLACEMENT_3D ( 'NONE', #14576, #8434, #1109 ) ;
#9622 = CARTESIAN_POINT ( 'NONE',  ( 232.5999999999999375, -34.83749999999999147, 103.0000000000000000 ) ) ;
#9623 = CARTESIAN_POINT ( 'NONE',  ( -83.77821517812500929, -34.22812499938549280, 102.3871387122750889 ) ) ;
#9624 = CARTESIAN_POINT ( 'NONE',  ( -82.39999999999999147, -32.61562499938548854, -103.1828516163667899 ) ) ;
#9625 = CARTESIAN_POINT ( 'NONE',  ( 85.15643035624999868, -32.42812499938548854, 101.5914258081833879 ) ) ;
#9626 = CARTESIAN_POINT ( 'NONE',  ( 81.02178482187500208, -31.45312499938549067, -102.3871387122750889 ) ) ;
#9627 = CARTESIAN_POINT ( 'NONE',  ( 229.8435696437499303, -33.29062499938547148, -50.00000000000011369 ) ) ;
#9628 = CARTESIAN_POINT ( 'NONE',  ( -83.77821517812500929, -33.77812499938548285, 102.3871387122750889 ) ) ;
#9629 = CARTESIAN_POINT ( 'NONE',  ( -79.64356964374999848, -34.07812499938548711, -99.99999999999998579 ) ) ;
#9630 = VERTEX_POINT ( 'NONE', #3119 ) ;
#9631 = CARTESIAN_POINT ( 'NONE',  ( 79.64356964374999848, -33.17812499938548854, 99.99999999999998579 ) ) ;
#9632 = CARTESIAN_POINT ( 'NONE',  ( -82.40000000000000568, -30.56250000000001066, 96.99999999999998579 ) ) ;
#9633 = AXIS2_PLACEMENT_3D ( 'NONE', #10412, #73, #1535 ) ;
#9634 = SHAPE_REPRESENTATION ( 'hex flange bolt small_iso_ISO 4162 - M5 x 20 x 20-N', ( #10540 ), #19229 ) ;
#9635 = CARTESIAN_POINT ( 'NONE',  ( -83.77821517812500929, -31.86562499938548498, 102.3871387122750889 ) ) ;
#9636 = CARTESIAN_POINT ( 'NONE',  ( -79.64356964375001269, -35.01562499938548711, 101.5914258081833879 ) ) ;
#9637 = EDGE_CURVE ( 'NONE', #9315, #2507, #14815, .T. ) ;
#9638 = CARTESIAN_POINT ( 'NONE',  ( -85.40000000000000568, -31.38749999999999929, 98.26794919243111792 ) ) ;
#9639 = VERTEX_POINT ( 'NONE', #10643 ) ;
#9640 = EDGE_CURVE ( 'NONE', #12903, #15041, #16457, .T. ) ;
#9641 = CARTESIAN_POINT ( 'NONE',  ( -82.39999999999999147, -32.58750000000000568, -96.53589838486223584 ) ) ;
#9642 = CARTESIAN_POINT ( 'NONE',  ( -82.40000000000001990, -32.53124999877097423, 103.0000000000000000 ) ) ;
#9643 = DIRECTION ( 'NONE',  ( 1.000000000000000000, 0.000000000000000000, 0.000000000000000000 ) ) ;
#9644 = CARTESIAN_POINT ( 'NONE',  ( -79.39999999999999147, -32.90624999877096712, 101.7320508075688537 ) ) ;
#9645 = CARTESIAN_POINT ( 'NONE',  ( 235.3564303562499447, -32.12812499938547717, 98.40857419181659793 ) ) ;
#9646 = CARTESIAN_POINT ( 'NONE',  ( -80.90000000000000568, -34.59768749875867400, 97.40192378864668399 ) ) ;
#9647 = EDGE_CURVE ( 'NONE', #9630, #7994, #11387, .T. ) ;
#9648 = CARTESIAN_POINT ( 'NONE',  ( 110.0000000000000000, 10.19999999999997620, -140.0000000000000000 ) ) ;
#9649 = CARTESIAN_POINT ( 'NONE',  ( 83.20384757729337366, -32.15759618943233278, 97.00000000000000000 ) ) ;
#9650 = PLANE ( 'NONE',  #8927 ) ;
#9651 = CARTESIAN_POINT ( 'NONE',  ( 79.64356964375001269, -30.96562499938548640, 98.40857419181659793 ) ) ;
#9652 = CARTESIAN_POINT ( 'NONE',  ( -69.99999999999998579, -35.00000000000000000, 150.0000000000000000 ) ) ;
#9653 = CARTESIAN_POINT ( 'NONE',  ( 83.77821517812500929, -31.67812499938548498, -97.61286128772489690 ) ) ;
#9654 = CARTESIAN_POINT ( 'NONE',  ( 82.40000000000000568, -34.61250000000001137, 102.9999999999999858 ) ) ;
#9655 = ORIENTED_EDGE ( 'NONE', *, *, #1928, .F. ) ;
#9656 = CARTESIAN_POINT ( 'NONE',  ( 80.90000000000000568, -31.89374999877096784, 102.5980762113533018 ) ) ;
#9657 = PRODUCT_CONTEXT ( 'NONE', #11203, 'mechanical' ) ;
#9658 = CARTESIAN_POINT ( 'NONE',  ( 235.3564303562499447, -31.41562499938548214, 101.5914258081833879 ) ) ;
#9659 = CARTESIAN_POINT ( 'NONE',  ( 232.5999999999999375, -33.29062499938547859, -46.81714838363331666 ) ) ;
#9660 = CARTESIAN_POINT ( 'NONE',  ( -85.15643035624999868, -33.70312499938548711, 101.5914258081833879 ) ) ;
#9661 = DIRECTION ( 'NONE',  ( 1.586032892321652482E-15, 1.000000000000000000, 3.469446951953616654E-16 ) ) ;
#9662 = ORIENTED_EDGE ( 'NONE', *, *, #11128, .F. ) ;
#9663 = ORIENTED_EDGE ( 'NONE', *, *, #9010, .T. ) ;
#9664 = CARTESIAN_POINT ( 'NONE',  ( -85.15643035625001289, -31.94062499938548427, -99.99999999999998579 ) ) ;
#9665 = DIRECTION ( 'NONE',  ( 0.000000000000000000, 0.000000000000000000, -1.000000000000000000 ) ) ;
#9666 = ORIENTED_EDGE ( 'NONE', *, *, #11037, .T. ) ;
#9667 = CARTESIAN_POINT ( 'NONE',  ( 79.64356964374998427, -33.66562499938548569, 98.40857419181659793 ) ) ;
#9668 = CARTESIAN_POINT ( 'NONE',  ( -79.39999999999999147, -32.90624999877096712, -98.26794919243113213 ) ) ;
#9669 = CARTESIAN_POINT ( 'NONE',  ( 82.39999999999999147, -33.71249999999999858, 103.4641016151377499 ) ) ;
#9670 = CARTESIAN_POINT ( 'NONE',  ( -79.39999999999999147, -31.98750000000000071, 98.26794919243110371 ) ) ;
#9671 = CARTESIAN_POINT ( 'NONE',  ( -82.39999999999999147, -32.98124999877096997, 103.4641016151377499 ) ) ;
#9672 = CARTESIAN_POINT ( 'NONE',  ( -79.39999999999999147, -34.21874999877096712, 99.99999999999998579 ) ) ;
#9673 = CARTESIAN_POINT ( 'NONE',  ( 85.23110191008899506, -34.99999999999998579, -99.14248198115983257 ) ) ;
#9674 = CARTESIAN_POINT ( 'NONE',  ( 231.0999999999999375, -34.06874999877096144, -52.59807621135342970 ) ) ;
#9675 = CARTESIAN_POINT ( 'NONE',  ( 80.90000000000000568, -30.54374999877096997, -97.40192378864668399 ) ) ;
#9676 = CARTESIAN_POINT ( 'NONE',  ( 235.3564303562499447, -33.10312499938547859, 101.5914258081833879 ) ) ;
#9677 = VERTEX_POINT ( 'NONE', #7618 ) ;
#9678 = CARTESIAN_POINT ( 'NONE',  ( 85.15643035625001289, -33.70312499938548711, -101.5914258081833879 ) ) ;
#9679 = CARTESIAN_POINT ( 'NONE',  ( 235.5999999999999943, -31.48124999877096286, 98.26794919243110371 ) ) ;
#9680 = CARTESIAN_POINT ( 'NONE',  ( 235.5999999999999943, -31.55624999877096215, -48.26794919243124582 ) ) ;
#9681 = ORIENTED_EDGE ( 'NONE', *, *, #17331, .F. ) ;
#9682 = DIRECTION ( 'NONE',  ( 0.000000000000000000, -0.000000000000000000, 1.000000000000000000 ) ) ;
#9683 = PLANE ( 'NONE',  #17089 ) ;
#9684 = CARTESIAN_POINT ( 'NONE',  ( 4.071447262713887127, 2.020725942163688504, 3.500000000000000000 ) ) ;
#9685 = ORIENTED_EDGE ( 'NONE', *, *, #11911, .T. ) ;
#9686 = CARTESIAN_POINT ( 'NONE',  ( 231.7961524227065979, -33.63615380933863008, 97.00000000000000000 ) ) ;
#9687 = LINE ( 'NONE', #903, #8483 ) ;
#9688 = ORIENTED_EDGE ( 'NONE', *, *, #18429, .F. ) ;
#9689 =( NAMED_UNIT ( * ) SI_UNIT ( $, .STERADIAN. ) SOLID_ANGLE_UNIT ( ) );
#9690 = CARTESIAN_POINT ( 'NONE',  ( 79.64356964375001269, -34.82812499938548711, -98.40857419181659793 ) ) ;
#9691 = CARTESIAN_POINT ( 'NONE',  ( 105.1999999999999744, -31.99999999999999289, 150.0000000000000000 ) ) ;
#9692 = CARTESIAN_POINT ( 'NONE',  ( -80.90000000000000568, -33.24374999877097281, 97.40192378864668399 ) ) ;
#9693 = CARTESIAN_POINT ( 'NONE',  ( -85.40000000000000568, -30.48749999999999716, 98.26794919243111792 ) ) ;
#9694 = CARTESIAN_POINT ( 'NONE',  ( 232.8256241621686797, -34.99999999999999289, -52.98025757954786741 ) ) ;
#9695 = CARTESIAN_POINT ( 'NONE',  ( 0.000000000000000000, 3.755786496842896592E-16, -3.499999999999999556 ) ) ;
#9696 = CARTESIAN_POINT ( 'NONE',  ( 85.40000000000000568, -33.99374999877097281, 99.99999999999998579 ) ) ;
#9697 = DIRECTION ( 'NONE',  ( 1.000000000000000000, 0.000000000000000000, 0.000000000000000000 ) ) ;
#9698 = CARTESIAN_POINT ( 'NONE',  ( -85.15643035624999868, -32.42812499938548854, 98.40857419181659793 ) ) ;
#9699 = CARTESIAN_POINT ( 'NONE',  ( -79.39999999999999147, -31.12500000000000355, 99.99999999999998579 ) ) ;
#9700 = ORIENTED_EDGE ( 'NONE', *, *, #6792, .F. ) ;
#9701 = CARTESIAN_POINT ( 'NONE',  ( 79.39999999999999147, -32.92500000000000426, 99.99999999999998579 ) ) ;
#9702 = CARTESIAN_POINT ( 'NONE',  ( -79.39999999999999147, -33.82500000000000284, 99.99999999999998579 ) ) ;
#9703 = EDGE_CURVE ( 'NONE', #13022, #1583, #18371, .T. ) ;
#9704 = EDGE_CURVE ( 'NONE', #15031, #13758, #10152, .T. ) ;
#9705 = LINE ( 'NONE', #9505, #5540 ) ;
#9706 = CARTESIAN_POINT ( 'NONE',  ( 232.5999999999999943, -32.16562499938547859, 96.81714838363319586 ) ) ;
#9707 = CARTESIAN_POINT ( 'NONE',  ( -83.77821517812500929, -34.82812499938548711, 97.61286128772489690 ) ) ;
#9708 = CARTESIAN_POINT ( 'NONE',  ( 229.8435696437499871, -34.71562499938548285, -48.40857419181671162 ) ) ;
#9709 = ORIENTED_EDGE ( 'NONE', *, *, #8289, .T. ) ;
#9710 = LINE ( 'NONE', #9905, #12541 ) ;
#9711 = CARTESIAN_POINT ( 'NONE',  ( 81.44948931429641448, -35.00000000000001421, 97.40655328406457159 ) ) ;
#9712 = CARTESIAN_POINT ( 'NONE',  ( 83.77821517812500929, -33.21562499938548285, 97.61286128772489690 ) ) ;
#9713 = CARTESIAN_POINT ( 'NONE',  ( -96.99999999999998579, -5.200000000000000178, 150.0000000000000000 ) ) ;
#9714 = ADVANCED_FACE ( 'NONE', ( #209 ), #6164, .F. ) ;
#9715 = CARTESIAN_POINT ( 'NONE',  ( 233.9782151781249411, -32.99062499938548143, -52.38713871227520968 ) ) ;
#9716 = CARTESIAN_POINT ( 'NONE',  ( -82.39999999999999147, -33.06562499938548427, 96.81714838363319586 ) ) ;
#9717 = CARTESIAN_POINT ( 'NONE',  ( 83.09162395290300651, -31.99999999999999289, 97.24830349208647817 ) ) ;
#9718 = CARTESIAN_POINT ( 'NONE',  ( 85.15643035624999868, -31.97812499938548925, 101.5914258081833879 ) ) ;
#9719 = CARTESIAN_POINT ( 'NONE',  ( 79.64356964375001269, -34.56562499938549138, -101.5914258081833879 ) ) ;
#9720 = CARTESIAN_POINT ( 'NONE',  ( 233.9782151781249411, -32.24062499938548143, -47.61286128772501769 ) ) ;
#9721 = CARTESIAN_POINT ( 'NONE',  ( -79.64356964374999848, -34.97812499938548569, 99.99999999999998579 ) ) ;
#9722 = CARTESIAN_POINT ( 'NONE',  ( -79.64356964375001269, -31.75312499938548427, -98.40857419181659793 ) ) ;
#9723 = ADVANCED_FACE ( 'NONE', ( #18085 ), #15138, .T. ) ;
#9724 = ORIENTED_EDGE ( 'NONE', *, *, #12745, .F. ) ;
#9725 = CARTESIAN_POINT ( 'NONE',  ( 79.64356964375001269, -33.59062499938548285, 101.5914258081833879 ) ) ;
#9726 = DIRECTION ( 'NONE',  ( 1.586032892321652285E-15, 1.000000000000000000, 0.000000000000000000 ) ) ;
#9727 = CARTESIAN_POINT ( 'NONE',  ( -85.40000000000000568, -33.18750000000000000, 98.26794919243111792 ) ) ;
#9728 = LINE ( 'NONE', #18525, #13014 ) ;
#9729 = CARTESIAN_POINT ( 'NONE',  ( -83.77821517812500929, -34.82812499938548711, 97.61286128772489690 ) ) ;
#9730 = DIRECTION ( 'NONE',  ( 0.000000000000000000, 0.000000000000000000, 1.000000000000000000 ) ) ;
#9731 = ORIENTED_EDGE ( 'NONE', *, *, #11016, .T. ) ;
#9732 = CARTESIAN_POINT ( 'NONE',  ( -79.39999999999999147, -34.72500000000000142, -99.99999999999998579 ) ) ;
#9733 = VECTOR ( 'NONE', #11489, 1000.000000000000000 ) ;
#9734 = AXIS2_PLACEMENT_3D ( 'NONE', #13302, #7061, #18992 ) ;
#9735 = CARTESIAN_POINT ( 'NONE',  ( -80.90000000000000568, -32.49374999877097281, 102.5980762113533018 ) ) ;
#9736 = CARTESIAN_POINT ( 'NONE',  ( 231.0999999999999375, -34.12499999999999289, -52.59807621135342970 ) ) ;
#9737 = CARTESIAN_POINT ( 'NONE',  ( -79.39999999999999147, -30.67106250001229029, 99.99999999999998579 ) ) ;
#9738 = CARTESIAN_POINT ( 'NONE',  ( -85.40000000000000568, -34.86018749875868394, 101.7320508075688679 ) ) ;
#9739 = CARTESIAN_POINT ( 'NONE',  ( 85.40000000000000568, -33.99374999877097281, -99.99999999999998579 ) ) ;
#9740 = CARTESIAN_POINT ( 'NONE',  ( 96.99999999999997158, -5.200000000000003730, 150.0000000000000000 ) ) ;
#9741 = DIRECTION ( 'NONE',  ( -0.000000000000000000, 0.000000000000000000, -1.000000000000000000 ) ) ;
#9742 = DIRECTION ( 'NONE',  ( -0.000000000000000000, -0.000000000000000000, -1.000000000000000000 ) ) ;
#9743 = CARTESIAN_POINT ( 'NONE',  ( 234.0999999999999375, -32.04374999877096286, 102.5980762113533018 ) ) ;
#9744 = CARTESIAN_POINT ( 'NONE',  ( 82.65333140691207348, -34.99995246259152992, 102.9892844631211943 ) ) ;
#9745 = CARTESIAN_POINT ( 'NONE',  ( 83.77821517812500929, -30.32812499938548711, -97.61286128772489690 ) ) ;
#9746 = CARTESIAN_POINT ( 'NONE',  ( 82.39999999999999147, -34.83749999999999858, -103.0000000000000000 ) ) ;
#9747 = EDGE_LOOP ( 'NONE', ( #1414, #2803, #231, #3203 ) ) ;
#9748 = DIRECTION ( 'NONE',  ( -1.000000000000000000, -0.000000000000000000, -0.000000000000000000 ) ) ;
#9749 = APPLICATION_PROTOCOL_DEFINITION ( 'draft international standard', 'automotive_design', 1998, #17572 ) ;
#9750 = CARTESIAN_POINT ( 'NONE',  ( 231.2217848218749339, -33.02812499938547575, 97.61286128772489690 ) ) ;
#9751 = CARTESIAN_POINT ( 'NONE',  ( 229.8435696437499871, -33.89062499938548001, -51.59142580818350865 ) ) ;
#9752 = CARTESIAN_POINT ( 'NONE',  ( -81.02178482187500208, -32.99062499938548854, 97.61286128772489690 ) ) ;
#9753 = CARTESIAN_POINT ( 'NONE',  ( 83.20384757729335945, -34.14240381056767148, 102.9999999999999716 ) ) ;
#9754 = EDGE_LOOP ( 'NONE', ( #6230, #10638, #19180, #8718, #16718 ) ) ;
#9755 = ADVANCED_FACE ( 'NONE', ( #13672 ), #18272, .T. ) ;
#9756 = CARTESIAN_POINT ( 'NONE',  ( -83.77821517812500929, -32.46562499938548285, -102.3871387122750889 ) ) ;
#9757 = CARTESIAN_POINT ( 'NONE',  ( 94.79999999999995453, -29.80000000000000071, -150.0000000000000000 ) ) ;
#9758 = ORIENTED_EDGE ( 'NONE', *, *, #13051, .T. ) ;
#9759 = CARTESIAN_POINT ( 'NONE',  ( 85.15643035625001289, -32.99062499938548854, 101.5914258081833879 ) ) ;
#9760 = CARTESIAN_POINT ( 'NONE',  ( -79.39999999999999147, -33.80624999877097281, -98.26794919243113213 ) ) ;
#9761 = AXIS2_PLACEMENT_3D ( 'NONE', #10939, #18378, #605 ) ;
#9762 = CARTESIAN_POINT ( 'NONE',  ( 83.90000000000000568, -34.12500000000000000, 102.5980762113533018 ) ) ;
#9763 = AXIS2_PLACEMENT_3D ( 'NONE', #7651, #9209, #16359 ) ;
#9764 = CARTESIAN_POINT ( 'NONE',  ( -83.90000000000000568, -34.57500000000000284, 97.40192378864668399 ) ) ;
#9765 = CARTESIAN_POINT ( 'NONE',  ( -79.39999999999999147, -32.00624999877096855, 101.7320508075688537 ) ) ;
#9766 = CARTESIAN_POINT ( 'NONE',  ( -81.02178482187500208, -32.35312499938548569, 102.3871387122750889 ) ) ;
#9767 = CARTESIAN_POINT ( 'NONE',  ( -82.39999999999999147, -32.27812499938548285, -96.81714838363319586 ) ) ;
#9768 = DIRECTION ( 'NONE',  ( 1.000000000000000000, 0.000000000000000000, 0.000000000000000000 ) ) ;
#9769 = CARTESIAN_POINT ( 'NONE',  ( -81.59615242270662350, -34.31115380933863435, 102.9999999999999716 ) ) ;
#9770 = CARTESIAN_POINT ( 'NONE',  ( 229.5999999999999375, -31.34999999999999432, 99.99999999999998579 ) ) ;
#9771 = EDGE_LOOP ( 'NONE', ( #17474, #14881, #8162, #14771 ) ) ;
#9772 = EDGE_CURVE ( 'NONE', #6366, #1665, #14827, .T. ) ;
#9773 = CARTESIAN_POINT ( 'NONE',  ( 79.64356964374998427, -32.57812499938548711, -98.40857419181659793 ) ) ;
#9774 =( NAMED_UNIT ( * ) SI_UNIT ( $, .STERADIAN. ) SOLID_ANGLE_UNIT ( ) );
#9775 = CARTESIAN_POINT ( 'NONE',  ( -82.40000000000001990, -32.30624999877097281, 97.00000000000000000 ) ) ;
#9776 = CARTESIAN_POINT ( 'NONE',  ( 229.5999999999999375, -31.74374999877096215, -50.00000000000011369 ) ) ;
#9777 = ORIENTED_EDGE ( 'NONE', *, *, #15604, .T. ) ;
#9778 = CARTESIAN_POINT ( 'NONE',  ( -83.04637810842696410, -35.00000000000000711, 97.04408774215416145 ) ) ;
#9779 = CARTESIAN_POINT ( 'NONE',  ( 112.9245130097707204, 10.26540512031890273, -150.0000000000000284 ) ) ;
#9780 = CARTESIAN_POINT ( 'NONE',  ( 235.2218879900010791, -34.99999999999999289, 100.8506536761482124 ) ) ;
#9781 = ORIENTED_EDGE ( 'NONE', *, *, #1639, .F. ) ;
#9782 = CARTESIAN_POINT ( 'NONE',  ( -85.40000000000000568, -34.03124999877096712, -101.7320508075688821 ) ) ;
#9783 = CARTESIAN_POINT ( 'NONE',  ( 4.132952817037867987, -2.031684012687262175, 3.518979934899752138 ) ) ;
#9784 = ORIENTED_EDGE ( 'NONE', *, *, #15435, .F. ) ;
#9785 = CARTESIAN_POINT ( 'NONE',  ( -96.99999999999998579, -29.80000000000000426, 150.0000000000000000 ) ) ;
#9786 = CARTESIAN_POINT ( 'NONE',  ( 79.39999999999999147, -32.43750000000000000, -98.26794919243110371 ) ) ;
#9787 = DIRECTION ( 'NONE',  ( 0.000000000000000000, 0.000000000000000000, 1.000000000000000000 ) ) ;
#9788 = CARTESIAN_POINT ( 'NONE',  ( -79.64356964375001269, -32.31562499938548427, 101.5914258081833879 ) ) ;
#9789 = CARTESIAN_POINT ( 'NONE',  ( -85.40000000000000568, -30.00000000000000355, 99.99999999999998579 ) ) ;
#9790 = UNCERTAINTY_MEASURE_WITH_UNIT (LENGTH_MEASURE( 1.000000000000000082E-05 ), #9330, 'distance_accuracy_value', 'NONE');
#9791 = CARTESIAN_POINT ( 'NONE',  ( -2.962450405966101950E-15, -29.79999999999996163, -103.0000000000000142 ) ) ;
#9792 = CARTESIAN_POINT ( 'NONE',  ( 231.7961524227065411, -33.05759618943232425, 102.9999999999999858 ) ) ;
#9793 = LINE ( 'NONE', #5504, #12043 ) ;
#9794 = CARTESIAN_POINT ( 'NONE',  ( -82.40000000000001990, -33.88124999877096855, 103.0000000000000000 ) ) ;
#9795 = CARTESIAN_POINT ( 'NONE',  ( -79.64356964374999848, -32.61562499938548854, 99.99999999999998579 ) ) ;
#9796 = DIRECTION ( 'NONE',  ( 1.000000000000000000, -1.387778780781445676E-15, -2.407412430484046130E-31 ) ) ;
#9797 = VERTEX_POINT ( 'NONE', #18175 ) ;
#9798 =( LENGTH_UNIT ( ) NAMED_UNIT ( * ) SI_UNIT ( .MILLI., .METRE. ) );
#9799 = LINE ( 'NONE', #13016, #10225 ) ;
#9800 = DIRECTION ( 'NONE',  ( -0.000000000000000000, -1.000000000000000000, -0.000000000000000000 ) ) ;
#9801 = CARTESIAN_POINT ( 'NONE',  ( 229.8435696437499303, -34.75312499938547717, 99.99999999999998579 ) ) ;
#9802 = CARTESIAN_POINT ( 'NONE',  ( -81.02178482187500208, -33.55312499938548854, 97.61286128772489690 ) ) ;
#9803 = CARTESIAN_POINT ( 'NONE',  ( 229.8435696437499303, -31.04062499938547859, -50.00000000000011369 ) ) ;
#9804 = ORIENTED_EDGE ( 'NONE', *, *, #16632, .F. ) ;
#9805 = CARTESIAN_POINT ( 'NONE',  ( -81.44948931429648553, -34.99999999999999289, -97.40655328406454316 ) ) ;
#9806 = CARTESIAN_POINT ( 'NONE',  ( -85.15643035625001289, -35.09062499938548285, 99.99999999999998579 ) ) ;
#9807 = CARTESIAN_POINT ( 'NONE',  ( -82.40000000000001990, -32.53124999877097423, 103.0000000000000000 ) ) ;
#9808 = CARTESIAN_POINT ( 'NONE',  ( 81.02178482187500208, -32.24062499938548854, 97.61286128772489690 ) ) ;
#9809 = FACE_OUTER_BOUND ( 'NONE', #3711, .T. ) ;
#9810 = CARTESIAN_POINT ( 'NONE',  ( 112.2864669432758831, 9.160276915580402246, -146.0372177658591681 ) ) ;
#9811 = B_SPLINE_CURVE_WITH_KNOTS ( 'NONE', 3,
 ( #1490, #4615, #7731, #7444 ),
 .UNSPECIFIED., .F., .F.,
 ( 4, 4 ),
 ( 0.002080789711329271950, 0.004173039763574512562 ),
 .UNSPECIFIED. ) ;
#9812 = CARTESIAN_POINT ( 'NONE',  ( -79.64356964374998427, -32.69062499938548427, 98.40857419181659793 ) ) ;
#9813 = CARTESIAN_POINT ( 'NONE',  ( -83.77821517812500929, -33.32812499938548711, -97.61286128772489690 ) ) ;
#9814 = CARTESIAN_POINT ( 'NONE',  ( 79.64356964374999848, -31.26562499938548356, 99.99999999999998579 ) ) ;
#9815 = CARTESIAN_POINT ( 'NONE',  ( 79.64356964375001269, -33.14062499938548711, -98.40857419181659793 ) ) ;
#9816 = CARTESIAN_POINT ( 'NONE',  ( 232.5999999999999375, -33.85312499938547859, -53.18285161636690361 ) ) ;
#9817 = CARTESIAN_POINT ( 'NONE',  ( -85.15643035625001289, -32.42812499938548854, 98.40857419181659793 ) ) ;
#9818 = CARTESIAN_POINT ( 'NONE',  ( 85.15643035624999868, -31.00312499938548072, -101.5914258081833879 ) ) ;
#9819 = ORIENTED_EDGE ( 'NONE', *, *, #15245, .F. ) ;
#9820 = CARTESIAN_POINT ( 'NONE',  ( 82.39999999999999147, -34.64062499938548711, 96.81714838363319586 ) ) ;
#9821 = CARTESIAN_POINT ( 'NONE',  ( 2.712762565639649015, -3.052587955997662306, -3.430618716626630871 ) ) ;
#9822 = CARTESIAN_POINT ( 'NONE',  ( -82.39999999999999147, -32.36250000000000426, 96.53589838486223584 ) ) ;
#9823 = CARTESIAN_POINT ( 'NONE',  ( -85.15643035625001289, -31.04062499938548569, 99.99999999999998579 ) ) ;
#9824 = CARTESIAN_POINT ( 'NONE',  ( -83.77821517812500929, -30.21562499938548285, 97.61286128772489690 ) ) ;
#9825 = DIRECTION ( 'NONE',  ( 1.000000000000000000, 0.000000000000000000, 0.000000000000000000 ) ) ;
#9826 = EDGE_LOOP ( 'NONE', ( #8113, #16896, #19121, #12200 ) ) ;
#9827 = CARTESIAN_POINT ( 'NONE',  ( -80.90000000000000568, -33.89999999999999858, -97.40192378864668399 ) ) ;
#9828 = PRODUCT_DEFINITION_SHAPE ( 'NONE', 'NONE',  #19323 ) ;
#9829 = DIRECTION ( 'NONE',  ( 1.000000000000000000, 0.000000000000000000, 0.000000000000000000 ) ) ;
#9830 = FACE_OUTER_BOUND ( 'NONE', #4776, .T. ) ;
#9831 = CARTESIAN_POINT ( 'NONE',  ( -80.90000000000000568, -30.14606250001229171, 97.40192378864668399 ) ) ;
#9832 = EDGE_CURVE ( 'NONE', #5766, #14052, #4799, .T. ) ;
#9833 = CARTESIAN_POINT ( 'NONE',  ( 3.880206590543030298, 3.396506438958510898, -1.117078279489021053 ) ) ;
#9834 = CARTESIAN_POINT ( 'NONE',  ( -83.41996205656103314, -35.00000000000000000, 97.17173842519740390 ) ) ;
#9835 = CARTESIAN_POINT ( 'NONE',  ( 234.0999999999999375, -32.99999999999999289, 102.5980762113533018 ) ) ;
#9836 = DIRECTION ( 'NONE',  ( -4.625929269271485791E-17, -1.000000000000000000, 0.000000000000000000 ) ) ;
#9837 = CARTESIAN_POINT ( 'NONE',  ( 81.02178482187500208, -31.30312499938548498, 102.3871387122750889 ) ) ;
#9838 = CARTESIAN_POINT ( 'NONE',  ( 232.5999999999999375, -29.99999999999999645, -53.00000000000012079 ) ) ;
#9839 = CARTESIAN_POINT ( 'NONE',  ( 232.5999999999999375, -29.99999999999999645, 103.0000000000000000 ) ) ;
#9840 = CARTESIAN_POINT ( 'NONE',  ( 81.02178482187500208, -33.10312499938548569, -97.61286128772489690 ) ) ;
#9841 = CARTESIAN_POINT ( 'NONE',  ( 79.39999999999999147, -32.90624999877096712, 98.26794919243113213 ) ) ;
#9842 = AXIS2_PLACEMENT_3D ( 'NONE', #6067, #17594, #10358 ) ;
#9843 = ORIENTED_EDGE ( 'NONE', *, *, #7314, .T. ) ;
#9844 = CARTESIAN_POINT ( 'NONE',  ( 80.90000000000000568, -30.99374999877096926, 102.5980762113533018 ) ) ;
#9845 = APPLICATION_PROTOCOL_DEFINITION ( 'draft international standard', 'automotive_design', 1998, #18425 ) ;
#9846 = EDGE_CURVE ( 'NONE', #2874, #7323, #3946, .T. ) ;
#9847 = CARTESIAN_POINT ( 'NONE',  ( 231.9680721332268547, -35.00000000000000711, -47.31096265646014842 ) ) ;
#9848 = CARTESIAN_POINT ( 'NONE',  ( 235.3564303562499447, -32.69062499938547717, -51.59142580818350865 ) ) ;
#9849 = ADVANCED_FACE ( 'NONE', ( #8860 ), #8954, .F. ) ;
#9850 = CARTESIAN_POINT ( 'NONE',  ( 233.4038475772933339, -34.31115380933863435, 102.9999999999999858 ) ) ;
#9851 = CARTESIAN_POINT ( 'NONE',  ( 82.39999999999999147, -34.83749999999999858, 97.00000000000000000 ) ) ;
#9852 = VERTEX_POINT ( 'NONE', #16105 ) ;
#9853 = CARTESIAN_POINT ( 'NONE',  ( -79.64356964375001269, -30.85312499938548569, -98.40857419181659793 ) ) ;
#9854 = EDGE_CURVE ( 'NONE', #7903, #9639, #716, .T. ) ;
#9855 = CARTESIAN_POINT ( 'NONE',  ( 113.0000000000000000, 10.39615242270649276, -145.9967928284264076 ) ) ;
#9856 = ORIENTED_EDGE ( 'NONE', *, *, #4234, .T. ) ;
#9857 = CARTESIAN_POINT ( 'NONE',  ( 82.39999999999999147, -33.96562499938548285, 103.1828516163667899 ) ) ;
#9858 = CARTESIAN_POINT ( 'NONE',  ( -79.64356964374999848, -30.47812499938548569, -99.99999999999998579 ) ) ;
#9859 = AXIS2_PLACEMENT_3D ( 'NONE', #15889, #13929, #10998 ) ;
#9860 = CARTESIAN_POINT ( 'NONE',  ( 79.39999999999999147, -34.23750000000000426, 101.7320508075688821 ) ) ;
#9861 = LINE ( 'NONE', #17382, #15364 ) ;
#9862 = CARTESIAN_POINT ( 'NONE',  ( -79.39999999999999147, -34.21874999877096712, 99.99999999999998579 ) ) ;
#9863 = CARTESIAN_POINT ( 'NONE',  ( -81.02178482187500208, -31.45312499938549067, 102.3871387122750889 ) ) ;
#9864 = LINE ( 'NONE', #6939, #11178 ) ;
#9865 = EDGE_CURVE ( 'NONE', #14886, #7672, #11933, .T. ) ;
#9866 = CARTESIAN_POINT ( 'NONE',  ( 235.2033360070650190, -31.99999999999999289, 101.4892189721556690 ) ) ;
#9867 = CARTESIAN_POINT ( 'NONE',  ( 229.5999999999999375, -31.83749999999999858, 98.26794919243111792 ) ) ;
#9868 = EDGE_LOOP ( 'NONE', ( #10911, #2964, #12425, #6334, #6425, #15448, #16842, #16103, #5702, #17657 ) ) ;
#9869 = CARTESIAN_POINT ( 'NONE',  ( 85.15643035625001289, -32.80312499938548854, -101.5914258081833879 ) ) ;
#9870 = FILL_AREA_STYLE_COLOUR ( '', #15848 ) ;
#9871 = CARTESIAN_POINT ( 'NONE',  ( 231.0999999999999375, -34.06874999877096144, 97.40192378864668399 ) ) ;
#9872 = CARTESIAN_POINT ( 'NONE',  ( 235.5999999999999943, -32.00624999877096144, -48.26794919243124582 ) ) ;
#9873 = ORIENTED_EDGE ( 'NONE', *, *, #12687, .T. ) ;
#9874 = AXIS2_PLACEMENT_3D ( 'NONE', #9131, #2981, #16570 ) ;
#9875 = DIRECTION ( 'NONE',  ( -0.000000000000000000, -1.000000000000000000, -0.000000000000000000 ) ) ;
#9876 = CARTESIAN_POINT ( 'NONE',  ( -85.15643035625001289, -31.97812499938548925, 98.40857419181659793 ) ) ;
#9877 = CARTESIAN_POINT ( 'NONE',  ( 1.411581201560190495E-15, 4.862606272033091592, -3.745885042887436622 ) ) ;
#9878 = ORIENTED_EDGE ( 'NONE', *, *, #18087, .F. ) ;
#9879 = DIRECTION ( 'NONE',  ( 1.000000000000000000, 0.000000000000000000, 0.000000000000000000 ) ) ;
#9880 = CARTESIAN_POINT ( 'NONE',  ( 4.175572532730931208, -2.061029303918050282, 3.569807470274392713 ) ) ;
#9881 = ORIENTED_EDGE ( 'NONE', *, *, #516, .F. ) ;
#9882 = CARTESIAN_POINT ( 'NONE',  ( 244.7999999999999545, -29.80000000000001492, -97.80000000000002558 ) ) ;
#9883 = CARTESIAN_POINT ( 'NONE',  ( 79.39999999999999147, -32.96250000000000568, -101.7320508075688537 ) ) ;
#9884 = EDGE_CURVE ( 'NONE', #5794, #6188, #16382, .T. ) ;
#9885 = DIRECTION ( 'NONE',  ( 7.222237291452149776E-32, -1.214306433183765213E-16, 1.000000000000000000 ) ) ;
#9886 = PRODUCT_DEFINITION_FORMATION_WITH_SPECIFIED_SOURCE ( 'ANY', '', #791, .NOT_KNOWN. ) ;
#9887 = CARTESIAN_POINT ( 'NONE',  ( -82.39999999999999147, -31.26562499938549067, 96.81714838363319586 ) ) ;
#9888 = CARTESIAN_POINT ( 'NONE',  ( -83.90000000000000568, -34.42106250001229739, 102.5980762113533018 ) ) ;
#9889 = CARTESIAN_POINT ( 'NONE',  ( 234.9631320699430432, -35.00000000000000000, -51.64628046580102705 ) ) ;
#9890 = DIRECTION ( 'NONE',  ( -1.586032892321652088E-15, -1.000000000000000000, 0.000000000000000000 ) ) ;
#9891 = CARTESIAN_POINT ( 'NONE',  ( 83.77821517812500929, -34.67812499938548854, -102.3871387122750889 ) ) ;
#9892 = EDGE_CURVE ( 'NONE', #10972, #13473, #6413, .T. ) ;
#9893 = CARTESIAN_POINT ( 'NONE',  ( 111.5000000000000142, 12.69999999999998508, 30.20101012677667285 ) ) ;
#9894 = CARTESIAN_POINT ( 'NONE',  ( 85.16220480609830190, -35.00000000000000000, 101.0868535717095682 ) ) ;
#9895 = ORIENTED_EDGE ( 'NONE', *, *, #458, .F. ) ;
#9896 = VECTOR ( 'NONE', #5697, 1000.000000000000000 ) ;
#9897 = CARTESIAN_POINT ( 'NONE',  ( 231.0999999999999375, -34.42499999999999716, -47.40192378864679768 ) ) ;
#9898 = DIRECTION ( 'NONE',  ( -0.000000000000000000, -1.000000000000000000, -0.000000000000000000 ) ) ;
#9899 = CARTESIAN_POINT ( 'NONE',  ( -82.40000000000000568, -33.43124999877096570, 102.9999999999999858 ) ) ;
#9900 = DIRECTION ( 'NONE',  ( 0.000000000000000000, 0.000000000000000000, -1.000000000000000000 ) ) ;
#9901 = CARTESIAN_POINT ( 'NONE',  ( -79.64356964374999848, -34.07812499938548711, 99.99999999999998579 ) ) ;
#9902 = CARTESIAN_POINT ( 'NONE',  ( 229.8435696437499871, -31.00312499938547361, -48.40857419181671162 ) ) ;
#9903 = CIRCLE ( 'NONE', #1476, 2.199999999999993516 ) ;
#9904 = ORIENTED_EDGE ( 'NONE', *, *, #3186, .F. ) ;
#9905 = CARTESIAN_POINT ( 'NONE',  ( 96.99999999999998579, 4.758098676964956264E-15, 150.0000000000000000 ) ) ;
#9906 = CARTESIAN_POINT ( 'NONE',  ( -85.15643035624999868, -33.70312499938548711, 101.5914258081833879 ) ) ;
#9907 = CARTESIAN_POINT ( 'NONE',  ( -85.40000000000000568, -30.43124999877096926, 98.26794919243111792 ) ) ;
#9908 = CARTESIAN_POINT ( 'NONE',  ( 79.39999999999999147, -30.67500000000000071, 99.99999999999998579 ) ) ;
#9909 = AXIS2_PLACEMENT_3D ( 'NONE', #5513, #11459, #14287 ) ;
#9910 = LINE ( 'NONE', #18900, #9292 ) ;
#9911 = CARTESIAN_POINT ( 'NONE',  ( 229.8435696437499587, -32.80312499938548143, -48.40857419181671162 ) ) ;
#9912 = CARTESIAN_POINT ( 'NONE',  ( -79.64356964374999848, -34.52812499938548285, 99.99999999999998579 ) ) ;
#9913 = CARTESIAN_POINT ( 'NONE',  ( -85.15643035625001289, -34.75312499938548427, -99.99999999999998579 ) ) ;
#9914 = CARTESIAN_POINT ( 'NONE',  ( 81.02178482187500208, -32.69062499938548427, 97.61286128772489690 ) ) ;
#9915 =( GEOMETRIC_REPRESENTATION_CONTEXT ( 3 ) GLOBAL_UNCERTAINTY_ASSIGNED_CONTEXT ( ( #12511 ) ) GLOBAL_UNIT_ASSIGNED_CONTEXT ( ( #15251, #16818, #4710 ) ) REPRESENTATION_CONTEXT ( 'NONE', 'WORKASPACE' ) );
#9916 = CARTESIAN_POINT ( 'NONE',  ( 79.64356964375001269, -34.94062499938549138, -98.40857419181659793 ) ) ;
#9917 = CARTESIAN_POINT ( 'NONE',  ( 233.9782151781249411, -33.44062499938547717, -52.38713871227520968 ) ) ;
#9918 = CARTESIAN_POINT ( 'NONE',  ( -81.02178482187500208, -32.24062499938548854, 102.3871387122750889 ) ) ;
#9919 = CARTESIAN_POINT ( 'NONE',  ( 85.15643035624999868, -31.45312499938548356, -101.5914258081833879 ) ) ;
#9920 = ORIENTED_EDGE ( 'NONE', *, *, #17017, .T. ) ;
#9921 = FACE_OUTER_BOUND ( 'NONE', #754, .T. ) ;
#9922 = VECTOR ( 'NONE', #6995, 1000.000000000000000 ) ;
#9923 = CARTESIAN_POINT ( 'NONE',  ( 3.522875095019493141, -2.820352903225631369, -3.598441714920572299 ) ) ;
#9924 = CARTESIAN_POINT ( 'NONE',  ( -85.40000000000000568, -34.53750000000000142, 98.26794919243111792 ) ) ;
#9925 = CARTESIAN_POINT ( 'NONE',  ( -81.02178482187500208, -33.14062499938548711, 102.3871387122750889 ) ) ;
#9926 = CARTESIAN_POINT ( 'NONE',  ( -82.39999999999999147, -30.70312499938548711, 96.81714838363319586 ) ) ;
#9927 = CARTESIAN_POINT ( 'NONE',  ( 4.071447262713887127, -2.020725942163688060, 3.500000000000000444 ) ) ;
#9928 = VECTOR ( 'NONE', #1647, 1000.000000000000000 ) ;
#9929 = AXIS2_PLACEMENT_3D ( 'NONE', #671, #15608, #2124 ) ;
#9930 = CARTESIAN_POINT ( 'NONE',  ( 99.99999999999994316, -29.80000000000000782, -150.0000000000000000 ) ) ;
#9931 = CARTESIAN_POINT ( 'NONE',  ( 232.5999999999999375, -34.83749999999999147, -47.00000000000011369 ) ) ;
#9932 = CARTESIAN_POINT ( 'NONE',  ( -83.90000000000000568, -30.82106250001229242, 102.5980762113533018 ) ) ;
#9933 = CARTESIAN_POINT ( 'NONE',  ( 3.948103430091329358, 2.682758828852234156, -2.353325403974033669 ) ) ;
#9934 = AXIS2_PLACEMENT_3D ( 'NONE', #1747, #15229, #15321 ) ;
#9935 = CARTESIAN_POINT ( 'NONE',  ( -80.90000000000000568, -32.79374999877096997, 97.40192378864668399 ) ) ;
#9936 = CARTESIAN_POINT ( 'NONE',  ( -82.39999999999999147, -30.70312499938548711, 96.81714838363319586 ) ) ;
#9937 = FACE_BOUND ( 'NONE', #8513, .T. ) ;
#9938 = CARTESIAN_POINT ( 'NONE',  ( 231.0723800503074870, -32.00000000000002132, 97.66884955414398917 ) ) ;
#9939 = DIRECTION ( 'NONE',  ( 0.000000000000000000, -2.001604010742465719E-15, -1.000000000000000000 ) ) ;
#9940 = CARTESIAN_POINT ( 'NONE',  ( 83.77821517812500929, -33.02812499938548285, -97.61286128772489690 ) ) ;
#9941 = AXIS2_PLACEMENT_3D ( 'NONE', #9021, #16734, #18115 ) ;
#9942 = CARTESIAN_POINT ( 'NONE',  ( 80.90000000000000568, -32.79374999877096997, 102.5980762113533018 ) ) ;
#9943 =( BOUNDED_CURVE ( )  B_SPLINE_CURVE ( 2, ( #11492, #3871, #10028, #11585, #14503, #8455, #8366, #11680, #2689 ),
 .UNSPECIFIED., .F., .F. ) 
 B_SPLINE_CURVE_WITH_KNOTS ( ( 3, 2, 2, 2, 3 ),
 ( 0.8541666666666665186, 0.8611111111111111605, 0.8750000000000000000, 0.8888888888888888395, 0.8958333333333333703 ),
 .UNSPECIFIED. ) 
 CURVE ( )  GEOMETRIC_REPRESENTATION_ITEM ( )  RATIONAL_B_SPLINE_CURVE ( ( 0.9330127018922194093, 0.9330127018922177440, 1.000000000000000000, 0.8660254037844387076, 1.000000000000000000, 0.8660254037844387076, 1.000000000000000000, 0.9330127018922187432, 0.9330127018922192983 ) ) 
 REPRESENTATION_ITEM ( '' )  );
#9944 = ORIENTED_EDGE ( 'NONE', *, *, #7495, .F. ) ;
#9945 = CARTESIAN_POINT ( 'NONE',  ( 79.39999999999999147, -32.83124999877097139, 101.7320508075688821 ) ) ;
#9946 = CONTEXT_DEPENDENT_SHAPE_REPRESENTATION ( #5224, #11231 ) ;
#9947 = CARTESIAN_POINT ( 'NONE',  ( 234.9210568921013476, -34.99999999999997868, -48.50261820439528293 ) ) ;
#9948 = CARTESIAN_POINT ( 'NONE',  ( 229.8435696437499871, -32.54062499938547859, -51.59142580818350865 ) ) ;
#9949 = EDGE_CURVE ( 'NONE', #2849, #15232, #6071, .T. ) ;
#9950 = ADVANCED_FACE ( 'NONE', ( #5661 ), #17667, .F. ) ;
#9951 = CARTESIAN_POINT ( 'NONE',  ( -82.40000000000000568, -30.00000000000000355, 99.99999999999998579 ) ) ;
#9952 = CARTESIAN_POINT ( 'NONE',  ( 3.951447005078455366, -3.704664227300106916, -0.5833333333333337034 ) ) ;
#9953 = ORIENTED_EDGE ( 'NONE', *, *, #17646, .T. ) ;
#9954 = CARTESIAN_POINT ( 'NONE',  ( -83.77821517812500929, -31.11562499938548498, -102.3871387122750889 ) ) ;
#9955 = CARTESIAN_POINT ( 'NONE',  ( 83.90000000000000568, -33.22500000000000142, 102.5980762113533018 ) ) ;
#9956 = ORIENTED_EDGE ( 'NONE', *, *, #4577, .F. ) ;
#9957 =( REPRESENTATION_RELATIONSHIP ('NONE','NONE', #14468, #16991 ) REPRESENTATION_RELATIONSHIP_WITH_TRANSFORMATION ( #8757 )SHAPE_REPRESENTATION_RELATIONSHIP( ) );
#9958 = CARTESIAN_POINT ( 'NONE',  ( 82.39999999999999147, -34.19062499938548427, 96.81714838363319586 ) ) ;
#9959 = CARTESIAN_POINT ( 'NONE',  ( -82.39999999999999147, -31.04062499938548569, -96.81714838363319586 ) ) ;
#9960 = CARTESIAN_POINT ( 'NONE',  ( 85.40000000000000568, -34.01250000000000284, 98.26794919243111792 ) ) ;
#9961 = LINE ( 'NONE', #15725, #15677 ) ;
#9962 = CARTESIAN_POINT ( 'NONE',  ( -82.39999999999999147, -34.55624999877096570, 96.53589838486223584 ) ) ;
#9963 = CARTESIAN_POINT ( 'NONE',  ( -79.64356964375001269, -30.96562499938548640, 101.5914258081833879 ) ) ;
#9964 = CARTESIAN_POINT ( 'NONE',  ( -83.77821517812500929, -33.81562499938548427, -102.3871387122750889 ) ) ;
#9965 = ADVANCED_FACE ( 'NONE', ( #1443 ), #2813, .T. ) ;
#9966 = DIRECTION ( 'NONE',  ( -0.000000000000000000, -1.000000000000000000, -0.000000000000000000 ) ) ;
#9967 = EDGE_CURVE ( 'NONE', #10928, #9562, #7310, .T. ) ;
#9968 = CARTESIAN_POINT ( 'NONE',  ( 79.39999999999999147, -31.10624999877097352, -101.7320508075688537 ) ) ;
#9969 = CARTESIAN_POINT ( 'NONE',  ( 232.5999999999999375, -31.68749999999999289, 103.4641016151377499 ) ) ;
#9970 = ORIENTED_EDGE ( 'NONE', *, *, #14175, .T. ) ;
#9971 = DIRECTION ( 'NONE',  ( -7.222237291452147586E-32, 1.214306433183764966E-16, -1.000000000000000000 ) ) ;
#9972 =( LENGTH_UNIT ( ) NAMED_UNIT ( * ) SI_UNIT ( .MILLI., .METRE. ) );
#9973 = CARTESIAN_POINT ( 'NONE',  ( 231.0999999999999375, -32.11874999877096570, 102.5980762113533018 ) ) ;
#9974 = CARTESIAN_POINT ( 'NONE',  ( 234.0999999999999375, -31.14374999877096428, -47.40192378864679768 ) ) ;
#9975 = CARTESIAN_POINT ( 'NONE',  ( 83.20384757729337366, -32.79240381056766296, 103.0000000000000000 ) ) ;
#9976 = CARTESIAN_POINT ( 'NONE',  ( -85.15643035625001289, -30.59062499938548285, 99.99999999999998579 ) ) ;
#9977 = ORIENTED_EDGE ( 'NONE', *, *, #7612, .T. ) ;
#9978 = ORIENTED_EDGE ( 'NONE', *, *, #9240, .T. ) ;
#9979 = CARTESIAN_POINT ( 'NONE',  ( -79.39999999999999147, -31.96874999877096712, 99.99999999999998579 ) ) ;
#9980 = CARTESIAN_POINT ( 'NONE',  ( 4.158413352280814657, -2.044871626972826650, 3.541821552872969292 ) ) ;
#9981 = ORIENTED_EDGE ( 'NONE', *, *, #4839, .F. ) ;
#9982 = CARTESIAN_POINT ( 'NONE',  ( 82.39999999999999147, -32.81250000000000000, -96.53589838486223584 ) ) ;
#9983 = FACE_OUTER_BOUND ( 'NONE', #18847, .T. ) ;
#9984 =( BOUNDED_CURVE ( )  B_SPLINE_CURVE ( 2, ( #12774, #3879, #11502, #4076, #2506, #8375, #7008, #2313, #10133 ),
 .UNSPECIFIED., .F., .F. ) 
 B_SPLINE_CURVE_WITH_KNOTS ( ( 3, 2, 2, 2, 3 ),
 ( 0.4791666666666666297, 0.4861111111111111049, 0.5000000000000000000, 0.5138888888888888395, 0.5208333333333334814 ),
 .UNSPECIFIED. ) 
 CURVE ( )  GEOMETRIC_REPRESENTATION_ITEM ( )  RATIONAL_B_SPLINE_CURVE ( ( 0.9330127018922194093, 0.9330127018922190762, 1.000000000000000000, 0.8660254037844387076, 1.000000000000000000, 0.8660254037844387076, 1.000000000000000000, 0.9330127018922177440, 0.9330127018922194093 ) ) 
 REPRESENTATION_ITEM ( '' )  );
#9985 = CARTESIAN_POINT ( 'NONE',  ( -85.15643035624999868, -32.46562499938548996, 101.5914258081833879 ) ) ;
#9986 = CARTESIAN_POINT ( 'NONE',  ( -85.40000000000000568, -31.35000000000000142, 99.99999999999998579 ) ) ;
#9987 = CARTESIAN_POINT ( 'NONE',  ( 246.9999999999999716, -29.80000000000000426, 150.0000000000000000 ) ) ;
#9988 =( NAMED_UNIT ( * ) PLANE_ANGLE_UNIT ( ) SI_UNIT ( $, .RADIAN. ) );
#9989 = CARTESIAN_POINT ( 'NONE',  ( 79.64356964374999848, -34.97812499938548569, -99.99999999999998579 ) ) ;
#9990 = CARTESIAN_POINT ( 'NONE',  ( 4.180231891692618440, 2.049421325483208101, 3.591231015387272851 ) ) ;
#9991 = CARTESIAN_POINT ( 'NONE',  ( -79.64356964374999848, -34.41562499938548569, 99.99999999999998579 ) ) ;
#9992 = DIRECTION ( 'NONE',  ( 0.000000000000000000, -1.000000000000000000, 0.000000000000000000 ) ) ;
#9993 = ORIENTED_EDGE ( 'NONE', *, *, #14393, .F. ) ;
#9994 = DIRECTION ( 'NONE',  ( 1.000000000000000000, 0.000000000000000000, 0.000000000000000000 ) ) ;
#9995 = CARTESIAN_POINT ( 'NONE',  ( 235.3995413886006247, -35.00000000000000000, 99.68825842091030154 ) ) ;
#9996 = PRODUCT_DEFINITION_SHAPE ( 'NONE', 'NONE',  #19336 ) ;
#9997 = CARTESIAN_POINT ( 'NONE',  ( 82.40000000000000568, -34.78124999877096712, 96.99999999999998579 ) ) ;
#9998 = CARTESIAN_POINT ( 'NONE',  ( -79.64356964374999848, -33.17812499938548854, 99.99999999999998579 ) ) ;
#9999 = CARTESIAN_POINT ( 'NONE',  ( 235.3564303562499447, -34.56562499938547717, -48.40857419181671162 ) ) ;
#10000 = ORIENTED_EDGE ( 'NONE', *, *, #6947, .F. ) ;
#10001 = EDGE_CURVE ( 'NONE', #17378, #16799, #1478, .T. ) ;
#10002 = CARTESIAN_POINT ( 'NONE',  ( -83.77821517812500929, -34.56562499938548427, 102.3871387122750889 ) ) ;
#10003 = DIRECTION ( 'NONE',  ( -0.000000000000000000, -1.000000000000000000, -0.000000000000000000 ) ) ;
#10004 = CARTESIAN_POINT ( 'NONE',  ( 79.64356964375001269, -34.82812499938548711, 101.5914258081833879 ) ) ;
#10005 = CARTESIAN_POINT ( 'NONE',  ( 0.3126073911696428675, 4.041451884327382338, -3.240528425403984455E-16 ) ) ;
#10006 = CARTESIAN_POINT ( 'NONE',  ( 233.9782151781249411, -31.64062499938547646, 97.61286128772489690 ) ) ;
#10007 = CARTESIAN_POINT ( 'NONE',  ( -82.39999999999999147, -34.16250000000000142, 97.00000000000000000 ) ) ;
#10008 = CARTESIAN_POINT ( 'NONE',  ( -79.64356964374998427, -32.76562499938548711, 101.5914258081833879 ) ) ;
#10009 = CARTESIAN_POINT ( 'NONE',  ( -85.15643035625001289, -33.81562499938548427, -98.40857419181659793 ) ) ;
#10010 = CARTESIAN_POINT ( 'NONE',  ( 85.15643035625001289, -33.29062499938547859, 99.99999999999998579 ) ) ;
#10011 = CARTESIAN_POINT ( 'NONE',  ( 81.02178482187500208, -34.60312499938549280, -102.3871387122750889 ) ) ;
#10012 = CARTESIAN_POINT ( 'NONE',  ( 229.8435696437499871, -33.25312499938547717, -48.40857419181671162 ) ) ;
#10013 = CARTESIAN_POINT ( 'NONE',  ( -79.64356964374998427, -33.92812499938548854, 98.40857419181659793 ) ) ;
#10014 = CARTESIAN_POINT ( 'NONE',  ( 83.77821517812500929, -31.41562499938548569, -102.3871387122750889 ) ) ;
#10015 = ORIENTED_EDGE ( 'NONE', *, *, #27, .T. ) ;
#10016 = CARTESIAN_POINT ( 'NONE',  ( 81.02178482187500208, -34.60312499938549280, 97.61286128772489690 ) ) ;
#10017 = EDGE_CURVE ( 'NONE', #16451, #13073, #6695, .T. ) ;
#10018 = CARTESIAN_POINT ( 'NONE',  ( 232.5999999999999091, -34.10624999877096286, -53.00000000000010658 ) ) ;
#10019 = CARTESIAN_POINT ( 'NONE',  ( -79.39999999999999147, -33.37500000000000000, 99.99999999999998579 ) ) ;
#10020 = CARTESIAN_POINT ( 'NONE',  ( -83.77821517812500929, -34.11562499938548854, 102.3871387122750889 ) ) ;
#10021 = CARTESIAN_POINT ( 'NONE',  ( -82.39999999999999147, -30.47812499938548569, 103.1828516163667899 ) ) ;
#10022 = ORIENTED_EDGE ( 'NONE', *, *, #14007, .F. ) ;
#10023 = CARTESIAN_POINT ( 'NONE',  ( 85.39999999999999147, -34.97364041986484295, 101.0919042218176287 ) ) ;
#10024 = CARTESIAN_POINT ( 'NONE',  ( 79.77811200999867935, -34.99999999999999289, -100.8506536761476013 ) ) ;
#10025 = CARTESIAN_POINT ( 'NONE',  ( 82.65333140691205926, -34.99995246259152282, -97.01071553687880566 ) ) ;
#10026 =( BOUNDED_CURVE ( )  B_SPLINE_CURVE ( 2, ( #9997, #15762, #14469, #8330, #13108, #6969, #16048, #14286, #5610 ),
 .UNSPECIFIED., .F., .F. ) 
 B_SPLINE_CURVE_WITH_KNOTS ( ( 3, 2, 2, 2, 3 ),
 ( 0.8125000000000001110, 0.8194444444444444198, 0.8333333333333333703, 0.8472222222222222099, 0.8530683953269213582 ),
 .UNSPECIFIED. ) 
 CURVE ( )  GEOMETRIC_REPRESENTATION_ITEM ( )  RATIONAL_B_SPLINE_CURVE ( ( 0.9330127018922194093, 0.9330127018922204085, 1.000000000000000000, 0.8660254037844387076, 1.000000000000000000, 0.8660254037844387076, 1.000000000000000000, 0.9436068149601996025, 0.9346881722405915305 ) ) 
 REPRESENTATION_ITEM ( '' )  );
#10027 = DIRECTION ( 'NONE',  ( -0.000000000000000000, -1.000000000000000000, -0.000000000000000000 ) ) ;
#10028 = CARTESIAN_POINT ( 'NONE',  ( -80.90000000000000568, -34.64999999999999858, 97.40192378864668399 ) ) ;
#10029 = B_SPLINE_CURVE_WITH_KNOTS ( 'NONE', 3,
 ( #3488, #9449, #15414, #13942, #581, #16976, #15711, #15899, #12962, #18933, #6830, #17176, #3779, #18642, #11305, #3976 ),
 .UNSPECIFIED., .F., .F.,
 ( 4, 3, 3, 3, 3, 4 ),
 ( 0.000000000000000000, 3.315506744709148100E-05, 6.608280158700110304E-05, 0.0001026520855292349047, 0.0001376952025668703029, 0.0001398064759194511696 ),
 .UNSPECIFIED. ) ;
#10030 = DIRECTION ( 'NONE',  ( -0.000000000000000000, -1.000000000000000000, -0.000000000000000000 ) ) ;
#10031 = DIRECTION ( 'NONE',  ( 1.000000000000000000, 0.000000000000000000, 0.000000000000000000 ) ) ;
#10032 = CARTESIAN_POINT ( 'NONE',  ( 79.64356964374999848, -30.47812499938548569, 99.99999999999998579 ) ) ;
#10033 = CARTESIAN_POINT ( 'NONE',  ( 99.99999999999994316, -29.80000000000001492, -130.0000000000000000 ) ) ;
#10034 = DIRECTION ( 'NONE',  ( 1.000000000000000000, -1.586032892321652285E-15, 0.000000000000000000 ) ) ;
#10035 = CARTESIAN_POINT ( 'NONE',  ( 79.64356964375001269, -34.49062499938548854, -98.40857419181659793 ) ) ;
#10036 = CARTESIAN_POINT ( 'NONE',  ( 244.7999999999999545, -35.00000000000000000, 147.7999999999999829 ) ) ;
#10037 = ADVANCED_FACE ( 'NONE', ( #7592 ), #10714, .T. ) ;
#10038 = ORIENTED_EDGE ( 'NONE', *, *, #9949, .T. ) ;
#10039 = CARTESIAN_POINT ( 'NONE',  ( 79.39999999999999147, -34.25624999877096855, 98.26794919243113213 ) ) ;
#10040 = CONTEXT_DEPENDENT_SHAPE_REPRESENTATION ( #18945, #12948 ) ;
#10041 = CARTESIAN_POINT ( 'NONE',  ( 105.1999999999999744, -31.99999999999999289, -100.0000000000000000 ) ) ;
#10042 = CARTESIAN_POINT ( 'NONE',  ( 229.8435696437499871, -32.01562499938548001, -48.40857419181671162 ) ) ;
#10043 = CARTESIAN_POINT ( 'NONE',  ( 82.40000000000000568, -34.61250000000001137, 102.9999999999999858 ) ) ;
#10044 = CARTESIAN_POINT ( 'NONE',  ( 231.7961524227065695, -32.79240381056765585, -53.00000000000011369 ) ) ;
#10045 = EDGE_LOOP ( 'NONE', ( #19051, #10902, #15908, #17831 ) ) ;
#10046 = CARTESIAN_POINT ( 'NONE',  ( -79.64356964375001269, -33.47812499938547859, -101.5914258081833879 ) ) ;
#10047 = CARTESIAN_POINT ( 'NONE',  ( -82.40000000000000568, -30.00000000000000355, -99.99999999999998579 ) ) ;
#10048 = ORIENTED_EDGE ( 'NONE', *, *, #11184, .F. ) ;
#10049 = CARTESIAN_POINT ( 'NONE',  ( -82.40000000000000568, -34.78124999877096712, -96.99999999999998579 ) ) ;
#10050 = CARTESIAN_POINT ( 'NONE',  ( -80.90000000000000568, -35.19374999877096855, -97.40192378864668399 ) ) ;
#10051 = CARTESIAN_POINT ( 'NONE',  ( 85.40000000000000568, -33.63750000000000284, 101.7320508075688679 ) ) ;
#10052 = CARTESIAN_POINT ( 'NONE',  ( 235.3564303562499447, -30.51562499938548001, 101.5914258081833879 ) ) ;
#10053 = CARTESIAN_POINT ( 'NONE',  ( -85.40000000000000568, -35.36739040097838682, 98.90809659374338025 ) ) ;
#10054 = CARTESIAN_POINT ( 'NONE',  ( -82.39999999999999147, -30.81562499938548427, 96.81714838363319586 ) ) ;
#10055 = CARTESIAN_POINT ( 'NONE',  ( -83.77821517812500929, -33.21562499938548285, -97.61286128772489690 ) ) ;
#10056 = VECTOR ( 'NONE', #17476, 1000.000000000000000 ) ;
#10057 = COLOUR_RGB ( '',0.8941176470588234615, 0.8941176470588234615, 0.8941176470588234615 ) ;
#10058 =( BOUNDED_CURVE ( )  B_SPLINE_CURVE ( 2, ( #1046, #5353, #11296, #13136, #7187, #2589, #8550, #4165, #18923 ),
 .UNSPECIFIED., .F., .F. ) 
 B_SPLINE_CURVE_WITH_KNOTS ( ( 3, 2, 2, 2, 3 ),
 ( 0.6458333333333332593, 0.6527777777777777901, 0.6666666666666666297, 0.6805555555555555802, 0.6875000000000000000 ),
 .UNSPECIFIED. ) 
 CURVE ( )  GEOMETRIC_REPRESENTATION_ITEM ( )  RATIONAL_B_SPLINE_CURVE ( ( 0.9330127018922192983, 0.9330127018922187432, 1.000000000000000000, 0.8660254037844387076, 1.000000000000000000, 0.8660254037844387076, 1.000000000000000000, 0.9330127018922194093, 0.9330127018922194093 ) ) 
 REPRESENTATION_ITEM ( '' )  );
#10059 = CYLINDRICAL_SURFACE ( 'NONE', #4277, 3.000000000000002665 ) ;
#10060 = CARTESIAN_POINT ( 'NONE',  ( 82.39999999999999147, -31.18124999877096926, -103.4641016151377499 ) ) ;
#10061 = CARTESIAN_POINT ( 'NONE',  ( 235.5999999999999943, -30.26249999999999218, 101.7320508075688537 ) ) ;
#10062 = ORIENTED_EDGE ( 'NONE', *, *, #1712, .F. ) ;
#10063 = CARTESIAN_POINT ( 'NONE',  ( 229.8435696437499303, -32.05312499938548143, -50.00000000000011369 ) ) ;
#10064 = CARTESIAN_POINT ( 'NONE',  ( 235.5999999999999375, -33.31874999877096144, 99.99999999999998579 ) ) ;
#10065 = CARTESIAN_POINT ( 'NONE',  ( 232.5999999999999375, -31.40624999877096712, -53.46410161513786363 ) ) ;
#10066 = CARTESIAN_POINT ( 'NONE',  ( 232.5999999999999375, -33.48749999999999716, -47.00000000000011369 ) ) ;
#10067 = CARTESIAN_POINT ( 'NONE',  ( -81.02178482187500208, -30.74062499938548498, 97.61286128772489690 ) ) ;
#10068 = VERTEX_POINT ( 'NONE', #471 ) ;
#10069 = ORIENTED_EDGE ( 'NONE', *, *, #11276, .T. ) ;
#10070 = CARTESIAN_POINT ( 'NONE',  ( 109.9999999999999432, -29.80000000000003268, -130.0000000000000000 ) ) ;
#10071 = VECTOR ( 'NONE', #4503, 1000.000000000000000 ) ;
#10072 = AXIS2_PLACEMENT_3D ( 'NONE', #3034, #9279, #11925 ) ;
#10073 = CARTESIAN_POINT ( 'NONE',  ( 233.4038475772933054, -34.36740381056765870, -47.00000000000011369 ) ) ;
#10074 = EDGE_LOOP ( 'NONE', ( #13785, #13981, #5400, #16404 ) ) ;
#10075 = EDGE_CURVE ( 'NONE', #9639, #6974, #7684, .T. ) ;
#10076 = CARTESIAN_POINT ( 'NONE',  ( 82.39999999999999147, -32.13749999999999574, -103.4641016151377499 ) ) ;
#10077 = CARTESIAN_POINT ( 'NONE',  ( 79.93183330737450376, -31.99999999999999289, -101.6855250459189648 ) ) ;
#10078 = CARTESIAN_POINT ( 'NONE',  ( -85.15643035624999868, -30.66562499938548569, 101.5914258081833879 ) ) ;
#10079 = CARTESIAN_POINT ( 'NONE',  ( -85.40000000000000568, -31.76249999999999929, 101.7320508075688679 ) ) ;
#10080 = CARTESIAN_POINT ( 'NONE',  ( -79.39999999999999147, -34.76250000000000284, -98.26794919243113213 ) ) ;
#10081 = EDGE_CURVE ( 'NONE', #1717, #9376, #16705, .T. ) ;
#10082 = FACE_OUTER_BOUND ( 'NONE', #1695, .T. ) ;
#10083 = DIRECTION ( 'NONE',  ( -1.000000000000000000, 1.387778780781445676E-15, 2.407412430484046130E-31 ) ) ;
#10084 = CARTESIAN_POINT ( 'NONE',  ( 94.79999999999995453, -29.80000000000000071, 150.0000000000000000 ) ) ;
#10085 = CIRCLE ( 'NONE', #12573, 2.649999999999982148 ) ;
#10086 = CARTESIAN_POINT ( 'NONE',  ( -83.90000000000000568, -34.36874999877097281, -97.40192378864668399 ) ) ;
#10087 = ORIENTED_EDGE ( 'NONE', *, *, #9148, .F. ) ;
#10088 = CARTESIAN_POINT ( 'NONE',  ( -85.15643035624999868, -31.97812499938548925, -101.5914258081833879 ) ) ;
#10089 = FACE_OUTER_BOUND ( 'NONE', #4667, .T. ) ;
#10090 = CARTESIAN_POINT ( 'NONE',  ( -79.39999999999999147, -33.35624999877096997, 101.7320508075688537 ) ) ;
#10091 = CARTESIAN_POINT ( 'NONE',  ( 2.000000000000000444, 3.464101615137754830, -3.142992957459231018 ) ) ;
#10092 = CARTESIAN_POINT ( 'NONE',  ( -79.64356964374999848, -34.52812499938548285, 99.99999999999998579 ) ) ;
#10093 = CARTESIAN_POINT ( 'NONE',  ( 79.39999999999999147, -32.51250000000000284, 98.26794919243113213 ) ) ;
#10094 = CARTESIAN_POINT ( 'NONE',  ( 233.9782151781249411, -32.69062499938547717, -47.61286128772501769 ) ) ;
#10095 =( BOUNDED_CURVE ( )  B_SPLINE_CURVE ( 2, ( #5266, #17274, #9942, #5362, #19026, #9841, #8559, #866, #5554 ),
 .UNSPECIFIED., .F., .T. ) 
 B_SPLINE_CURVE_WITH_KNOTS ( ( 3, 2, 2, 2, 3 ),
 ( 0.4374999999999999445, 0.4444444444444444198, 0.4583333333333333148, 0.4722222222222222099, 0.4791666666666666297 ),
 .UNSPECIFIED. ) 
 CURVE ( )  GEOMETRIC_REPRESENTATION_ITEM ( )  RATIONAL_B_SPLINE_CURVE ( ( 0.9330127018922192983, 0.9330127018922187432, 1.000000000000000000, 0.8660254037844387076, 1.000000000000000000, 0.8660254037844387076, 1.000000000000000000, 0.9330127018922196314, 0.9330127018922194093 ) ) 
 REPRESENTATION_ITEM ( '' )  );
#10096 = EDGE_CURVE ( 'NONE', #12925, #3019, #9339, .T. ) ;
#10097 = EDGE_LOOP ( 'NONE', ( #6535, #401, #18385, #6527, #5288 ) ) ;
#10098 = CARTESIAN_POINT ( 'NONE',  ( -82.39999999999999147, -33.17812499938548854, 103.1828516163667899 ) ) ;
#10099 = EDGE_CURVE ( 'NONE', #13209, #5719, #15019, .T. ) ;
#10100 = CARTESIAN_POINT ( 'NONE',  ( -83.41996205656103314, -35.00000000000000000, -102.8282615748025108 ) ) ;
#10101 = CARTESIAN_POINT ( 'NONE',  ( 85.15643035625001289, -34.19062499938548427, 99.99999999999998579 ) ) ;
#10102 = CARTESIAN_POINT ( 'NONE',  ( -83.20384757729335945, -32.60759618943233562, 102.9999999999999858 ) ) ;
#10103 = CARTESIAN_POINT ( 'NONE',  ( 232.5999999999999375, -32.50312499938547717, 96.81714838363319586 ) ) ;
#10104 = CARTESIAN_POINT ( 'NONE',  ( 233.9782151781249411, -32.09062499938547575, -52.38713871227520968 ) ) ;
#10105 = CARTESIAN_POINT ( 'NONE',  ( -79.39999999999999147, -30.63750000000000284, 98.26794919243110371 ) ) ;
#10106 = CARTESIAN_POINT ( 'NONE',  ( -85.15643035625001289, -32.99062499938548854, -101.5914258081833879 ) ) ;
#10107 = CARTESIAN_POINT ( 'NONE',  ( 0.3126073911696462537, -4.041451884327388555, -1.676097590879904329E-16 ) ) ;
#10108 = CARTESIAN_POINT ( 'NONE',  ( 85.15643035625001289, -35.20312499938548711, -99.99999999999998579 ) ) ;
#10109 = ADVANCED_FACE ( 'NONE', ( #18149 ), #12375, .F. ) ;
#10110 = CARTESIAN_POINT ( 'NONE',  ( 229.5999999999999375, -31.31249999999998934, -48.26794919243123161 ) ) ;
#10111 = CARTESIAN_POINT ( 'NONE',  ( -82.39999999999999147, -32.50312499938548427, 96.81714838363319586 ) ) ;
#10112 = DIRECTION ( 'NONE',  ( -0.000000000000000000, -0.000000000000000000, -1.000000000000000000 ) ) ;
#10113 = ORIENTED_EDGE ( 'NONE', *, *, #17821, .F. ) ;
#10114 = CARTESIAN_POINT ( 'NONE',  ( 84.51155386534844638, -35.25364837475780888, 101.7717924772919957 ) ) ;
#10115 = FACE_BOUND ( 'NONE', #11951, .T. ) ;
#10116 = CARTESIAN_POINT ( 'NONE',  ( -82.39999999999999147, -33.71249999999999858, 96.53589838486223584 ) ) ;
#10117 = CARTESIAN_POINT ( 'NONE',  ( -85.15643035624999868, -33.32812499938548001, 98.40857419181659793 ) ) ;
#10118 = CARTESIAN_POINT ( 'NONE',  ( -82.39999999999999147, -31.15312499938548640, 96.81714838363319586 ) ) ;
#10119 = ORIENTED_EDGE ( 'NONE', *, *, #16544, .T. ) ;
#10120 = CARTESIAN_POINT ( 'NONE',  ( 99.99999999999994316, -29.80000000000001492, -130.0000000000000000 ) ) ;
#10121 = CARTESIAN_POINT ( 'NONE',  ( 229.8435696437499587, -33.25312499938547717, 101.5914258081833879 ) ) ;
#10122 = CARTESIAN_POINT ( 'NONE',  ( 84.70388354820681798, -35.00002705695767702, 101.9214814096700934 ) ) ;
#10123 = CARTESIAN_POINT ( 'NONE',  ( -80.90000000000000568, -30.29606250001229384, 102.5980762113533018 ) ) ;
#10124 = EDGE_CURVE ( 'NONE', #9797, #2832, #19223, .T. ) ;
#10125 = CARTESIAN_POINT ( 'NONE',  ( 2.499999999999999556, 0.000000000000000000, 3.469446951953614189E-15 ) ) ;
#10126 = CARTESIAN_POINT ( 'NONE',  ( 99.99999999999997158, -29.80000000000000071, 150.0000000000000000 ) ) ;
#10127 = CARTESIAN_POINT ( 'NONE',  ( -83.90000000000000568, -34.51874999877097139, 97.40192378864668399 ) ) ;
#10128 = CARTESIAN_POINT ( 'NONE',  ( -82.40000000000001990, -32.75624999877096855, 97.00000000000000000 ) ) ;
#10129 = CARTESIAN_POINT ( 'NONE',  ( 82.39999999999999147, -33.51562499938548001, 103.1828516163667899 ) ) ;
#10130 = FACE_OUTER_BOUND ( 'NONE', #6369, .T. ) ;
#10131 = CARTESIAN_POINT ( 'NONE',  ( 232.5999999999999375, -34.78124999877096002, -47.00000000000011369 ) ) ;
#10132 = CARTESIAN_POINT ( 'NONE',  ( 81.02178482187500208, -34.60312499938549280, -102.3871387122750889 ) ) ;
#10133 = CARTESIAN_POINT ( 'NONE',  ( -82.39999999999999147, -33.20624999877097849, 97.00000000000000000 ) ) ;
#10134 = ORIENTED_EDGE ( 'NONE', *, *, #5825, .T. ) ;
#10135 = CARTESIAN_POINT ( 'NONE',  ( 82.39999999999999147, -33.65624999877096712, 103.4641016151377499 ) ) ;
#10136 = CARTESIAN_POINT ( 'NONE',  ( 235.3564303562499447, -35.01562499938548001, 101.5914258081833879 ) ) ;
#10137 = CARTESIAN_POINT ( 'NONE',  ( 229.8435696437499871, -34.79062499938547859, -51.59142580818350865 ) ) ;
#10138 = DIRECTION ( 'NONE',  ( 0.000000000000000000, 0.000000000000000000, -1.000000000000000000 ) ) ;
#10139 = CARTESIAN_POINT ( 'NONE',  ( -84.85538848574856274, -35.00000000000001421, -101.7224313860082674 ) ) ;
#10140 = ORIENTED_EDGE ( 'NONE', *, *, #9647, .T. ) ;
#10141 = CARTESIAN_POINT ( 'NONE',  ( -81.02178482187500208, -34.79062499938548569, -102.3871387122750889 ) ) ;
#10142 = CARTESIAN_POINT ( 'NONE',  ( 79.39999999999999147, -32.38124999877096855, 101.7320508075688963 ) ) ;
#10143 = ORIENTED_EDGE ( 'NONE', *, *, #15198, .F. ) ;
#10144 = CARTESIAN_POINT ( 'NONE',  ( -79.64356964375001269, -30.44062499938548783, -101.5914258081833879 ) ) ;
#10145 =( BOUNDED_SURFACE ( )  B_SPLINE_SURFACE ( 1, 2, ( 
 ( #14990, #3159, #16361, #4348, #17927, #1613, #10495, #6106, #15084, #13228, #2877, #10308, #5723, #8834, #16460, #19101, #10399, #7469, #7562, #9120, #2971, #14791, #4536, #155, #12054, #4644, #7181, #19202, #1417, #19303, #11673, #10211, #10594, #11862, #16174, #1519, #17829, #13130, #17637, #2783, #8926, #4441, #8736, #14690, #56, #5817, #11766, #6006, #12535, #13713, #18507, #18124, #10877, #11068, #15475, #1991, #16848, #1794, #7758, #9612, #17038, #18410, #5030, #14001, #9409, #3648, #2087, #7653, #13899, #1701, #18314, #13609, #12348, #4739, #1892, #16940, #5125, #354, #3552, #7947, #6493, #447, #10684, #7850, #15374, #8043, #3452, #16743, #537, #639, #12442, #10970, #251, #12156, #6208, #16652, #9509, #3255, #10780, #6394, #9211, #13805, #6588, #15177, #12251, #6301, #18219, #4837, #3356, #9313, #15277, #4933, #8242, #12737, #15955, #9999, #2372, #5614, #3936, #9708, #17521, #18993, #3741, #8143, #2187, #15669, #1104, #2278, #4041, #11362, #17136, #18606, #6972, #14473, #18895 ),
 ( #14192, #18705, #829, #2559, #17327, #6788, #5221, #12924, #7062, #5515, #11461, #5325, #5422, #926, #11263, #17231, #3835, #17429, #14095, #18797, #15865, #8523, #11559, #9902, #9803, #1021, #13021, #4134, #15574, #734, #15765, #8333, #14289, #6688, #11170, #12632, #6882, #12831, #2472, #8429, #14381, #8618, #7447, #11842, #11746, #6087, #13404, #8814, #1591, #1206, #3046, #7540, #2761, #13498, #7163, #19278, #137, #4514, #10379, #5894, #10185, #16148, #18006, #12034, #36, #5986, #9008, #17810, #10094, #10472, #16052, #2951, #2655, #7349, #14568, #1397, #13112, #10288, #11938, #19083, #8716, #17909, #16341, #14866, #14770, #5701, #16248, #4420, #16437, #8904, #5793, #1493, #14969, #11653, #17614, #4229, #14670, #1305, #7253, #13207, #19179, #17713, #13304, #4328, #2857, #18292, #1683, #15156, #12135, #16828, #6566, #7635, #618, #7925, #3330, #16630, #1773, #5011, #18391, #10758, #13978, #12326, #18105, #12514, #8019, #4716, #16538, #10574, #10661, #9485, #4618, #13589, #3138, #13876, #9290 ) ),
 .UNSPECIFIED., .F., .F., .F. ) 
 B_SPLINE_SURFACE_WITH_KNOTS ( ( 2, 2 ),
 ( 3, 2, 2, 2, 2, 2, 2, 2, 2, 2, 2, 2, 2, 2, 2, 2, 2, 2, 2, 2, 2, 2, 2, 2, 2, 2, 2, 2, 2, 2, 2, 2, 2, 2, 2, 2, 2, 2, 2, 2, 2, 2, 2, 2, 2, 2, 2, 2, 2, 2, 2, 2, 2, 2, 2, 2, 2, 2, 2, 2, 2, 2, 2, 2, 2, 2, 2, 3 ),
 ( 0.000000000000000000, 1.000000000000000000 ),
 ( 0.000000000000000000, 0.01388888888888888812, 0.02777777777777777624, 0.04166666666666666435, 0.05555555555555555247, 0.06944444444444444753, 0.08333333333333332871, 0.09722222222222222376, 0.1111111111111111049, 0.1250000000000000000, 0.1388888888888888951, 0.1527777777777777901, 0.1666666666666666574, 0.1805555555555555525, 0.1944444444444444475, 0.2083333333333333426, 0.2222222222222222099, 0.2361111111111111049, 0.2500000000000000000, 0.2638888888888888951, 0.2777777777777777901, 0.2916666666666666852, 0.3055555555555555802, 0.3194444444444444198, 0.3333333333333333148, 0.3472222222222222099, 0.3611111111111111049, 0.3750000000000000000, 0.3888888888888888951, 0.4027777777777777901, 0.4166666666666666852, 0.4305555555555555802, 0.4444444444444444198, 0.4583333333333333148, 0.4722222222222222099, 0.4861111111111111049, 0.5000000000000000000, 0.5138888888888888395, 0.5277777777777777901, 0.5416666666666666297, 0.5555555555555555802, 0.5694444444444444198, 0.5833333333333333703, 0.5972222222222222099, 0.6111111111111111605, 0.6250000000000000000, 0.6388888888888888395, 0.6527777777777777901, 0.6666666666666666297, 0.6805555555555555802, 0.6944444444444444198, 0.7083333333333333703, 0.7222222222222222099, 0.7361111111111111605, 0.7500000000000000000, 0.7638888888888888395, 0.7777777777777777901, 0.7916666666666666297, 0.8055555555555555802, 0.8194444444444444198, 0.8333333333333333703, 0.8472222222222222099, 0.8611111111111111605, 0.8750000000000000000, 0.8888888888888888395, 0.9027777777777777901, 0.9166666666666666297, 0.9258785565094813652 ),
 .UNSPECIFIED. ) 
 GEOMETRIC_REPRESENTATION_ITEM ( )  RATIONAL_B_SPLINE_SURFACE ( (
 ( 1.000000000000000000, 0.8660254037844387076, 1.000000000000000000, 0.8660254037844387076, 1.000000000000000000, 0.8660254037844387076, 1.000000000000000000, 0.8660254037844387076, 1.000000000000000000, 0.8660254037844387076, 1.000000000000000000, 0.8660254037844387076, 1.000000000000000000, 0.8660254037844387076, 1.000000000000000000, 0.8660254037844387076, 1.000000000000000000, 0.8660254037844387076, 1.000000000000000000, 0.8660254037844387076, 1.000000000000000000, 0.8660254037844387076, 1.000000000000000000, 0.8660254037844387076, 1.000000000000000000, 0.8660254037844387076, 1.000000000000000000, 0.8660254037844387076, 1.000000000000000000, 0.8660254037844387076, 1.000000000000000000, 0.8660254037844387076, 1.000000000000000000, 0.8660254037844387076, 1.000000000000000000, 0.8660254037844387076, 1.000000000000000000, 0.8660254037844387076, 1.000000000000000000, 0.8660254037844387076, 1.000000000000000000, 0.8660254037844387076, 1.000000000000000000, 0.8660254037844387076, 1.000000000000000000, 0.8660254037844387076, 1.000000000000000000, 0.8660254037844387076, 1.000000000000000000, 0.8660254037844387076, 1.000000000000000000, 0.8660254037844387076, 1.000000000000000000, 0.8660254037844387076, 1.000000000000000000, 0.8660254037844387076, 1.000000000000000000, 0.8660254037844387076, 1.000000000000000000, 0.8660254037844387076, 1.000000000000000000, 0.8660254037844387076, 1.000000000000000000, 0.8660254037844387076, 1.000000000000000000, 0.8660254037844387076, 1.000000000000000000, 0.8660254037844387076, 1.000000000000000000, 0.8660254037844387076, 1.000000000000000000, 0.8660254037844387076, 1.000000000000000000, 0.8660254037844387076, 1.000000000000000000, 0.8660254037844387076, 1.000000000000000000, 0.8660254037844387076, 1.000000000000000000, 0.8660254037844387076, 1.000000000000000000, 0.8660254037844387076, 1.000000000000000000, 0.8660254037844387076, 1.000000000000000000, 0.8660254037844387076, 1.000000000000000000, 0.8660254037844387076, 1.000000000000000000, 0.8660254037844387076, 1.000000000000000000, 0.8660254037844387076, 1.000000000000000000, 0.8660254037844387076, 1.000000000000000000, 0.8660254037844387076, 1.000000000000000000, 0.8660254037844387076, 1.000000000000000000, 0.8660254037844387076, 1.000000000000000000, 0.8660254037844387076, 1.000000000000000000, 0.8660254037844387076, 1.000000000000000000, 0.8660254037844387076, 1.000000000000000000, 0.8660254037844387076, 1.000000000000000000, 0.8660254037844387076, 1.000000000000000000, 0.8660254037844387076, 1.000000000000000000, 0.8660254037844387076, 1.000000000000000000, 0.8660254037844387076, 1.000000000000000000, 0.8660254037844387076, 1.000000000000000000, 0.8660254037844387076, 1.000000000000000000, 0.8660254037844387076, 1.000000000000000000, 0.8660254037844387076, 1.000000000000000000, 0.8660254037844387076, 1.000000000000000000, 0.8660254037844387076, 1.000000000000000000, 0.8660254037844387076, 1.000000000000000000, 0.8660254037844387076, 1.000000000000000000, 0.9111405360107203144, 0.9401542295229963209),
 ( 1.000000000000000000, 0.8660254037844387076, 1.000000000000000000, 0.8660254037844387076, 1.000000000000000000, 0.8660254037844387076, 1.000000000000000000, 0.8660254037844387076, 1.000000000000000000, 0.8660254037844387076, 1.000000000000000000, 0.8660254037844387076, 1.000000000000000000, 0.8660254037844387076, 1.000000000000000000, 0.8660254037844387076, 1.000000000000000000, 0.8660254037844387076, 1.000000000000000000, 0.8660254037844387076, 1.000000000000000000, 0.8660254037844387076, 1.000000000000000000, 0.8660254037844387076, 1.000000000000000000, 0.8660254037844387076, 1.000000000000000000, 0.8660254037844387076, 1.000000000000000000, 0.8660254037844387076, 1.000000000000000000, 0.8660254037844387076, 1.000000000000000000, 0.8660254037844387076, 1.000000000000000000, 0.8660254037844387076, 1.000000000000000000, 0.8660254037844387076, 1.000000000000000000, 0.8660254037844387076, 1.000000000000000000, 0.8660254037844387076, 1.000000000000000000, 0.8660254037844387076, 1.000000000000000000, 0.8660254037844387076, 1.000000000000000000, 0.8660254037844387076, 1.000000000000000000, 0.8660254037844387076, 1.000000000000000000, 0.8660254037844387076, 1.000000000000000000, 0.8660254037844387076, 1.000000000000000000, 0.8660254037844387076, 1.000000000000000000, 0.8660254037844387076, 1.000000000000000000, 0.8660254037844387076, 1.000000000000000000, 0.8660254037844387076, 1.000000000000000000, 0.8660254037844387076, 1.000000000000000000, 0.8660254037844387076, 1.000000000000000000, 0.8660254037844387076, 1.000000000000000000, 0.8660254037844387076, 1.000000000000000000, 0.8660254037844387076, 1.000000000000000000, 0.8660254037844387076, 1.000000000000000000, 0.8660254037844387076, 1.000000000000000000, 0.8660254037844387076, 1.000000000000000000, 0.8660254037844387076, 1.000000000000000000, 0.8660254037844387076, 1.000000000000000000, 0.8660254037844387076, 1.000000000000000000, 0.8660254037844387076, 1.000000000000000000, 0.8660254037844387076, 1.000000000000000000, 0.8660254037844387076, 1.000000000000000000, 0.8660254037844387076, 1.000000000000000000, 0.8660254037844387076, 1.000000000000000000, 0.8660254037844387076, 1.000000000000000000, 0.8660254037844387076, 1.000000000000000000, 0.8660254037844387076, 1.000000000000000000, 0.8660254037844387076, 1.000000000000000000, 0.8660254037844387076, 1.000000000000000000, 0.8660254037844387076, 1.000000000000000000, 0.8660254037844387076, 1.000000000000000000, 0.8660254037844387076, 1.000000000000000000, 0.8660254037844387076, 1.000000000000000000, 0.8660254037844387076, 1.000000000000000000, 0.8660254037844387076, 1.000000000000000000, 0.8660254037844387076, 1.000000000000000000, 0.8660254037844387076, 1.000000000000000000, 0.8660254037844387076, 1.000000000000000000, 0.8660254037844387076, 1.000000000000000000, 0.8660254037844387076, 1.000000000000000000, 0.8660254037844387076, 1.000000000000000000, 0.8660254037844387076, 1.000000000000000000, 0.8660254037844387076, 1.000000000000000000, 0.9111405360107203144, 0.9401542295229963209) ) ) 
 REPRESENTATION_ITEM ( '' )  SURFACE ( )  );
#10146 = CARTESIAN_POINT ( 'NONE',  ( -80.90000000000000568, -31.89374999877096784, -102.5980762113533018 ) ) ;
#10147 = CARTESIAN_POINT ( 'NONE',  ( 233.9782151781249411, -30.55312499938548143, 102.3871387122750889 ) ) ;
#10148 = CARTESIAN_POINT ( 'NONE',  ( -85.40000000000000568, -34.89374999877097139, 99.99999999999998579 ) ) ;
#10149 = CARTESIAN_POINT ( 'NONE',  ( -85.15643035624999868, -30.29062499938548925, 98.40857419181659793 ) ) ;
#10150 = CARTESIAN_POINT ( 'NONE',  ( -84.05108659120797654, -32.00820041275124339, -102.2295963284774842 ) ) ;
#10151 = DIRECTION ( 'NONE',  ( 1.000000000000000000, 0.000000000000000000, -0.000000000000000000 ) ) ;
#10152 = CIRCLE ( 'NONE', #15772, 5.199999999999996625 ) ;
#10153 = LINE ( 'NONE', #2619, #10824 ) ;
#10154 = CARTESIAN_POINT ( 'NONE',  ( 79.39999999999999147, -31.51874999877096784, -99.99999999999998579 ) ) ;
#10155 = CARTESIAN_POINT ( 'NONE',  ( 234.0999999999999375, -32.09999999999999432, 102.5980762113533018 ) ) ;
#10156 = ORIENTED_EDGE ( 'NONE', *, *, #9098, .F. ) ;
#10157 = CARTESIAN_POINT ( 'NONE',  ( 83.77821517812500929, -34.26562499938548711, -97.61286128772489690 ) ) ;
#10158 = CARTESIAN_POINT ( 'NONE',  ( 235.5999999999999943, -32.38124999877096144, 98.26794919243110371 ) ) ;
#10159 = CARTESIAN_POINT ( 'NONE',  ( 234.0999999999999375, -33.39374999877096428, -47.40192378864679768 ) ) ;
#10160 = CARTESIAN_POINT ( 'NONE',  ( -79.64356964374998427, -32.12812499938548427, 98.40857419181659793 ) ) ;
#10161 = ORIENTED_EDGE ( 'NONE', *, *, #5795, .F. ) ;
#10162 = VERTEX_POINT ( 'NONE', #3387 ) ;
#10163 = CARTESIAN_POINT ( 'NONE',  ( -79.39999999999999147, -32.02500000000000568, 99.99999999999998579 ) ) ;
#10164 = CIRCLE ( 'NONE', #17966, 3.000000000000002665 ) ;
#10165 = CARTESIAN_POINT ( 'NONE',  ( 113.0000000000000142, 10.19999999999997264, -150.0000000000000000 ) ) ;
#10166 = ORIENTED_EDGE ( 'NONE', *, *, #13150, .F. ) ;
#10167 = DIRECTION ( 'NONE',  ( 0.000000000000000000, 0.000000000000000000, 1.000000000000000000 ) ) ;
#10168 = CARTESIAN_POINT ( 'NONE',  ( 113.0000000000000000, 15.19999999999996732, -136.6833752096445380 ) ) ;
#10169 = CARTESIAN_POINT ( 'NONE',  ( 84.44763168836730927, -32.00000000000000711, -101.8452947671444093 ) ) ;
#10170 = CARTESIAN_POINT ( 'NONE',  ( -85.15643035625001289, -32.50312499938548427, 99.99999999999998579 ) ) ;
#10171 = CARTESIAN_POINT ( 'NONE',  ( -79.39999999999999147, -32.43750000000000000, 98.26794919243110371 ) ) ;
#10172 = CARTESIAN_POINT ( 'NONE',  ( 235.5999999999999375, -32.41874999877096286, -50.00000000000011369 ) ) ;
#10173 = SURFACE_STYLE_USAGE ( .BOTH. , #17316 ) ;
#10174 = CARTESIAN_POINT ( 'NONE',  ( -84.69814140657796031, -35.23021079535107702, 98.07164679703846843 ) ) ;
#10175 = CARTESIAN_POINT ( 'NONE',  ( 84.75088379146879447, -34.99999999999999289, 98.39201219457936531 ) ) ;
#10176 = CARTESIAN_POINT ( 'NONE',  ( 231.2217848218749339, -30.51562499938548001, 102.3871387122750889 ) ) ;
#10177 = EDGE_LOOP ( 'NONE', ( #14397, #14420, #13230, #12759 ) ) ;
#10178 = CARTESIAN_POINT ( 'NONE',  ( -83.77821517812500929, -30.51562499938548711, -97.61286128772489690 ) ) ;
#10179 = CYLINDRICAL_SURFACE ( 'NONE', #1485, 3.000000000000002665 ) ;
#10180 = ADVANCED_FACE ( 'NONE', ( #4963 ), #7973, .F. ) ;
#10181 = CARTESIAN_POINT ( 'NONE',  ( -4.236525694536558362, 2.416953475386465211, -3.751298745799836354 ) ) ;
#10182 = CARTESIAN_POINT ( 'NONE',  ( 231.2217848218749339, -34.82812499938548001, 97.61286128772489690 ) ) ;
#10183 = CARTESIAN_POINT ( 'NONE',  ( -85.15643035625001289, -31.94062499938548427, 99.99999999999998579 ) ) ;
#10184 = PLANE ( 'NONE',  #17227 ) ;
#10185 = CARTESIAN_POINT ( 'NONE',  ( 229.8435696437499303, -32.39062499938548001, -50.00000000000011369 ) ) ;
#10186 = EDGE_CURVE ( 'NONE', #8568, #12074, #2350, .T. ) ;
#10187 = EDGE_CURVE ( 'NONE', #11798, #9344, #13923, .T. ) ;
#10188 = VERTEX_POINT ( 'NONE', #665 ) ;
#10189 = ORIENTED_EDGE ( 'NONE', *, *, #14158, .T. ) ;
#10190 = CARTESIAN_POINT ( 'NONE',  ( -83.90000000000000568, -31.72500000000000142, 102.5980762113533018 ) ) ;
#10191 = CARTESIAN_POINT ( 'NONE',  ( -79.64356964375001269, -34.82812499938548711, 98.40857419181659793 ) ) ;
#10192 = CARTESIAN_POINT ( 'NONE',  ( 85.40000000000000568, -32.15624999877096712, -101.7320508075688821 ) ) ;
#10193 = CARTESIAN_POINT ( 'NONE',  ( 79.64356964375001269, -34.45312499938548711, 98.40857419181659793 ) ) ;
#10194 = CARTESIAN_POINT ( 'NONE',  ( 82.40000000000000568, -33.93750000000000711, -102.9999999999999858 ) ) ;
#10195 = CARTESIAN_POINT ( 'NONE',  ( 229.8435696437499871, -31.52812499938547575, 98.40857419181659793 ) ) ;
#10196 = CARTESIAN_POINT ( 'NONE',  ( 232.5999999999999943, -34.30312499938547433, -53.18285161636690361 ) ) ;
#10197 = B_SPLINE_CURVE_WITH_KNOTS ( 'NONE', 3,
 ( #6356, #18275, #12404, #1948, #7906, #499 ),
 .UNSPECIFIED., .F., .F.,
 ( 4, 2, 4 ),
 ( 0.002365888236228001588, 0.003551327329835089319, 0.004736766423442177049 ),
 .UNSPECIFIED. ) ;
#10198 = CARTESIAN_POINT ( 'NONE',  ( 105.1999999999999602, -32.00000000000000711, -97.80000000000002558 ) ) ;
#10199 = FACE_OUTER_BOUND ( 'NONE', #16877, .T. ) ;
#10200 = ADVANCED_FACE ( 'NONE', ( #2495 ), #853, .T. ) ;
#10201 = CARTESIAN_POINT ( 'NONE',  ( 83.77821517812500929, -31.41562499938548569, -102.3871387122750889 ) ) ;
#10202 = CARTESIAN_POINT ( 'NONE',  ( 232.5999999999999375, -34.97812499938547859, -46.81714838363331666 ) ) ;
#10203 = EDGE_CURVE ( 'NONE', #15015, #14886, #15935, .T. ) ;
#10204 = CARTESIAN_POINT ( 'NONE',  ( -85.15643035625001289, -34.19062499938548427, 99.99999999999998579 ) ) ;
#10205 = CARTESIAN_POINT ( 'NONE',  ( 81.02178482187500208, -31.64062499938548356, -97.61286128772489690 ) ) ;
#10206 = VECTOR ( 'NONE', #7720, 1000.000000000000000 ) ;
#10207 = EDGE_CURVE ( 'NONE', #10587, #11515, #18732, .T. ) ;
#10208 = ORIENTED_EDGE ( 'NONE', *, *, #4005, .F. ) ;
#10209 = CARTESIAN_POINT ( 'NONE',  ( 79.64356964375001269, -34.04062499938549280, 101.5914258081833879 ) ) ;
#10210 = CARTESIAN_POINT ( 'NONE',  ( -80.90000000000000568, -34.59374999877096712, 97.40192378864668399 ) ) ;
#10211 = CARTESIAN_POINT ( 'NONE',  ( 235.3564303562499447, -31.41562499938548214, -48.40857419181671162 ) ) ;
#10212 = CARTESIAN_POINT ( 'NONE',  ( -81.02178482187500208, -34.49062499938548854, 102.3871387122750889 ) ) ;
#10213 = ORIENTED_EDGE ( 'NONE', *, *, #10081, .F. ) ;
#10214 = CARTESIAN_POINT ( 'NONE',  ( -83.20384757729334524, -30.54240381056766651, 96.99999999999997158 ) ) ;
#10215 = CARTESIAN_POINT ( 'NONE',  ( 235.3564303562499447, -33.02812499938547575, 98.40857419181659793 ) ) ;
#10216 = FACE_OUTER_BOUND ( 'NONE', #16028, .T. ) ;
#10217 = CARTESIAN_POINT ( 'NONE',  ( -85.40000000000000568, -33.59606250001230165, 99.99999999999998579 ) ) ;
#10218 = AXIS2_PLACEMENT_3D ( 'NONE', #7891, #1927, #5159 ) ;
#10219 = CARTESIAN_POINT ( 'NONE',  ( 4.086262629614029862, 4.082406995609984435, 0.07093633357110337712 ) ) ;
#10220 = CARTESIAN_POINT ( 'NONE',  ( 83.20395887649171129, -35.00000000000000711, -102.6365808225363878 ) ) ;
#10221 = CARTESIAN_POINT ( 'NONE',  ( -79.64356964375001269, -32.12812499938548427, 98.40857419181659793 ) ) ;
#10222 = CYLINDRICAL_SURFACE ( 'NONE', #17042, 3.000000000000002665 ) ;
#10223 = CARTESIAN_POINT ( 'NONE',  ( 81.02178482187500208, -32.35312499938548569, 97.61286128772489690 ) ) ;
#10224 = DIRECTION ( 'NONE',  ( 0.000000000000000000, 0.000000000000000000, -1.000000000000000000 ) ) ;
#10225 = VECTOR ( 'NONE', #9898, 1000.000000000000000 ) ;
#10226 = CARTESIAN_POINT ( 'NONE',  ( -82.39999999999999147, -33.48750000000000426, -97.00000000000000000 ) ) ;
#10227 = CARTESIAN_POINT ( 'NONE',  ( 79.64356964374999848, -34.52812499938548285, -99.99999999999998579 ) ) ;
#10228 = CARTESIAN_POINT ( 'NONE',  ( -81.02178482187500208, -31.30312499938548498, -102.3871387122750889 ) ) ;
#10229 = ORIENTED_EDGE ( 'NONE', *, *, #15817, .T. ) ;
#10230 = ADVANCED_FACE ( 'NONE', ( #2400, #9830 ), #567, .T. ) ;
#10231 = CARTESIAN_POINT ( 'NONE',  ( 79.39999999999999147, -34.18124999877097281, 101.7320508075688821 ) ) ;
#10232 = ITEM_DEFINED_TRANSFORMATION ( 'NONE', 'NONE', #16727,  #10540 ) ;
#10233 = CARTESIAN_POINT ( 'NONE',  ( 229.8435696437499871, -33.81562499938547717, 101.5914258081833879 ) ) ;
#10234 = EDGE_CURVE ( 'NONE', #18009, #5078, #14316, .T. ) ;
#10235 = DIRECTION ( 'NONE',  ( -0.000000000000000000, -1.000000000000000000, -0.000000000000000000 ) ) ;
#10236 = AXIS2_PLACEMENT_3D ( 'NONE', #15001, #4653, #16471 ) ;
#10237 = CARTESIAN_POINT ( 'NONE',  ( -82.39999999999999147, -34.97812499938547859, 103.1828516163667899 ) ) ;
#10238 = CARTESIAN_POINT ( 'NONE',  ( 83.30522522564156418, -32.00000000000000000, 102.6670244572690365 ) ) ;
#10239 = VERTEX_POINT ( 'NONE', #6909 ) ;
#10240 = CARTESIAN_POINT ( 'NONE',  ( -83.77821517812500929, -33.36562499938548854, -102.3871387122750889 ) ) ;
#10241 = CARTESIAN_POINT ( 'NONE',  ( 4.197478902586992966, -0.8524102783748346290, -3.505063281295504041 ) ) ;
#10242 = EDGE_LOOP ( 'NONE', ( #4913, #8280, #16363, #2927 ) ) ;
#10243 = CARTESIAN_POINT ( 'NONE',  ( 231.7961524227065695, -33.69240381056765443, -53.00000000000010658 ) ) ;
#10244 = VECTOR ( 'NONE', #3089, 1000.000000000000000 ) ;
#10245 = EDGE_CURVE ( 'NONE', #13073, #14240, #3365, .T. ) ;
#10246 = CARTESIAN_POINT ( 'NONE',  ( -82.39999999999999147, -35.00624999877097565, -103.4641016151377499 ) ) ;
#10247 = CARTESIAN_POINT ( 'NONE',  ( -83.30522522562117160, -32.00000000000001421, -102.6670244572773498 ) ) ;
#10248 = CARTESIAN_POINT ( 'NONE',  ( -79.39999999999999147, -31.96874999877096712, -99.99999999999998579 ) ) ;
#10249 = CARTESIAN_POINT ( 'NONE',  ( 229.8435696437499871, -31.11562499938547788, 101.5914258081833879 ) ) ;
#10250 = CARTESIAN_POINT ( 'NONE',  ( -85.40000000000000568, -34.03124999877096712, 98.26794919243111792 ) ) ;
#10251 = CARTESIAN_POINT ( 'NONE',  ( -79.64356964375001269, -33.21562499938548996, 101.5914258081833879 ) ) ;
#10252 = CARTESIAN_POINT ( 'NONE',  ( -85.15643035625001289, -34.15312499938548285, -98.40857419181659793 ) ) ;
#10253 = CARTESIAN_POINT ( 'NONE',  ( 0.000000000000000000, 0.000000000000000000, 0.000000000000000000 ) ) ;
#10254 = VECTOR ( 'NONE', #5644, 1000.000000000000000 ) ;
#10255 = CARTESIAN_POINT ( 'NONE',  ( -81.59615242270662350, -34.31115380933863435, -96.99999999999998579 ) ) ;
#10256 = CARTESIAN_POINT ( 'NONE',  ( 85.40000000000000568, -31.25624999877096855, -101.7320508075688679 ) ) ;
#10257 = CARTESIAN_POINT ( 'NONE',  ( 229.5999999999999375, -34.01249999999999574, 101.7320508075688679 ) ) ;
#10258 = VERTEX_POINT ( 'NONE', #9931 ) ;
#10259 = DIRECTION ( 'NONE',  ( 1.586032892321652285E-15, 1.000000000000000000, 0.000000000000000000 ) ) ;
#10260 = CARTESIAN_POINT ( 'NONE',  ( 231.0999999999999375, -32.56874999877096144, 102.5980762113533018 ) ) ;
#10261 = CARTESIAN_POINT ( 'NONE',  ( 231.0999999999999375, -34.36874999877096570, -47.40192378864679768 ) ) ;
#10262 = CARTESIAN_POINT ( 'NONE',  ( -83.77821517812500929, -33.81562499938548427, 97.61286128772489690 ) ) ;
#10263 = ORIENTED_EDGE ( 'NONE', *, *, #15080, .T. ) ;
#10264 = ORIENTED_EDGE ( 'NONE', *, *, #11037, .F. ) ;
#10265 = CARTESIAN_POINT ( 'NONE',  ( -84.28136653320154892, -32.00000000000001421, 97.98546077809197641 ) ) ;
#10266 = AXIS2_PLACEMENT_3D ( 'NONE', #3035, #6270, #8996 ) ;
#10267 =( BOUNDED_CURVE ( )  B_SPLINE_CURVE ( 2, ( #17024, #9792, #11055, #15360, #627, #2263, #3822, #524, #8232 ),
 .UNSPECIFIED., .F., .F. ) 
 B_SPLINE_CURVE_WITH_KNOTS ( ( 3, 2, 2, 2, 3 ),
 ( 0.5625000000000002220, 0.5694444444444444198, 0.5833333333333333703, 0.5972222222222222099, 0.6041666666666667407 ),
 .UNSPECIFIED. ) 
 CURVE ( )  GEOMETRIC_REPRESENTATION_ITEM ( )  RATIONAL_B_SPLINE_CURVE ( ( 0.9330127018922194093, 0.9330127018922215187, 1.000000000000000000, 0.8660254037844387076, 1.000000000000000000, 0.8660254037844387076, 1.000000000000000000, 0.9330127018922187432, 0.9330127018922192983 ) ) 
 REPRESENTATION_ITEM ( '' )  );
#10268 = CARTESIAN_POINT ( 'NONE',  ( 229.5999999999999375, -34.94999999999999574, 99.99999999999998579 ) ) ;
#10269 = PLANE ( 'NONE',  #7859 ) ;
#10270 = ORIENTED_EDGE ( 'NONE', *, *, #412, .F. ) ;
#10271 = CARTESIAN_POINT ( 'NONE',  ( 232.5999999999999375, -34.61249999999999716, -53.00000000000011369 ) ) ;
#10272 = CYLINDRICAL_SURFACE ( 'NONE', #8185, 3.000000000000002665 ) ;
#10273 = CARTESIAN_POINT ( 'NONE',  ( -82.40000000000000568, -34.38749999999999574, 102.9999999999999858 ) ) ;
#10274 = CARTESIAN_POINT ( 'NONE',  ( -79.64356964375001269, -34.94062499938549138, 98.40857419181659793 ) ) ;
#10275 = CARTESIAN_POINT ( 'NONE',  ( -85.40000000000000568, -32.28750000000000142, 98.26794919243111792 ) ) ;
#10276 = CARTESIAN_POINT ( 'NONE',  ( 231.0723800503075154, -31.99999999999999289, -52.33115044585625242 ) ) ;
#10277 = CARTESIAN_POINT ( 'NONE',  ( 82.41196654184807358, -35.00000000000000711, 102.9991646027828835 ) ) ;
#10278 = CARTESIAN_POINT ( 'NONE',  ( 84.59935209580183368, -34.99999999999999289, 98.20719995774791755 ) ) ;
#10279 = CARTESIAN_POINT ( 'NONE',  ( 244.7999999999999545, -29.80000000000000426, 150.0000000000000000 ) ) ;
#10280 = ORIENTED_EDGE ( 'NONE', *, *, #9358, .T. ) ;
#10281 = SURFACE_SIDE_STYLE ('',( #17705 ) ) ;
#10282 = CARTESIAN_POINT ( 'NONE',  ( -81.02178482187500208, -35.05312499938548854, -97.61286128772489690 ) ) ;
#10283 = DIRECTION ( 'NONE',  ( -0.000000000000000000, -0.000000000000000000, -1.000000000000000000 ) ) ;
#10284 = CARTESIAN_POINT ( 'NONE',  ( -82.40000000000000568, -34.78124999877096712, 102.9999999999999858 ) ) ;
#10285 = CARTESIAN_POINT ( 'NONE',  ( 229.5999999999999375, -34.40624999877096002, 101.7320508075688821 ) ) ;
#10286 = CARTESIAN_POINT ( 'NONE',  ( -82.39999999999999147, -30.70312499938548711, 96.81714838363319586 ) ) ;
#10287 = CARTESIAN_POINT ( 'NONE',  ( 111.0000000000000000, 10.19999999999997620, -142.6499999999999773 ) ) ;
#10288 = CARTESIAN_POINT ( 'NONE',  ( 235.3564303562499447, -33.02812499938547575, -51.59142580818350865 ) ) ;
#10289 = ORIENTED_EDGE ( 'NONE', *, *, #8745, .F. ) ;
#10290 = EDGE_LOOP ( 'NONE', ( #2711, #9441, #12970, #2611 ) ) ;
#10291 = FACE_OUTER_BOUND ( 'NONE', #15973, .T. ) ;
#10292 = CARTESIAN_POINT ( 'NONE',  ( -82.39999999999999147, -30.78750000000000497, 103.4641016151377499 ) ) ;
#10293 = CARTESIAN_POINT ( 'NONE',  ( -82.39999999999999147, -32.36250000000000426, 96.99999999999998579 ) ) ;
#10294 = CARTESIAN_POINT ( 'NONE',  ( 82.39999999999999147, -34.75312499938549138, 103.1828516163667899 ) ) ;
#10295 = CARTESIAN_POINT ( 'NONE',  ( -82.40000000000000568, -30.00000000000000355, 99.99999999999998579 ) ) ;
#10296 = CARTESIAN_POINT ( 'NONE',  ( 232.5999999999999375, -32.27812499938547575, 103.1828516163667899 ) ) ;
#10297 = CARTESIAN_POINT ( 'NONE',  ( 231.2217848218749339, -33.21562499938547575, -47.61286128772501769 ) ) ;
#10298 = CARTESIAN_POINT ( 'NONE',  ( 232.5999999999999375, -29.99999999999999645, 99.99999999999998579 ) ) ;
#10299 = CARTESIAN_POINT ( 'NONE',  ( 79.64356964375001269, -33.55312499938548854, 98.40857419181659793 ) ) ;
#10300 = EDGE_CURVE ( 'NONE', #484, #6637, #15451, .T. ) ;
#10301 = CARTESIAN_POINT ( 'NONE',  ( 79.64356964375001269, -31.22812499938548925, -98.40857419181659793 ) ) ;
#10302 = B_SPLINE_CURVE_WITH_KNOTS ( 'NONE', 3,
 ( #425, #18289, #2250, #3620, #709, #12323 ),
 .UNSPECIFIED., .F., .F.,
 ( 4, 2, 4 ),
 ( 0.002365888236227967761, 0.003551327329835077609, 0.004736766423442186590 ),
 .UNSPECIFIED. ) ;
#10303 = CARTESIAN_POINT ( 'NONE',  ( 233.9782151781249411, -34.94062499938547717, -47.61286128772501769 ) ) ;
#10304 = CARTESIAN_POINT ( 'NONE',  ( -83.77821517812500929, -34.71562499938548285, 97.61286128772489690 ) ) ;
#10305 = CARTESIAN_POINT ( 'NONE',  ( 79.64356964375001269, -33.47812499938547859, -98.40857419181659793 ) ) ;
#10306 = ORIENTED_EDGE ( 'NONE', *, *, #17283, .T. ) ;
#10307 = CARTESIAN_POINT ( 'NONE',  ( -82.40000000000000568, -34.78124999877096712, 102.9999999999999858 ) ) ;
#10308 = CARTESIAN_POINT ( 'NONE',  ( 229.8435696437499871, -30.66562499938547859, -48.40857419181671162 ) ) ;
#10309 = CARTESIAN_POINT ( 'NONE',  ( -83.77821517812500929, -32.31562499938548427, 102.3871387122750889 ) ) ;
#10310 = ORIENTED_EDGE ( 'NONE', *, *, #17948, .F. ) ;
#10312 = EDGE_CURVE ( 'NONE', #17007, #5783, #16965, .T. ) ;
#10311 = CARTESIAN_POINT ( 'NONE',  ( -79.39999999999999147, -32.96250000000000568, 101.7320508075688537 ) ) ;
#10313 = EDGE_CURVE ( 'NONE', #13743, #15900, #5249, .T. ) ;
#10314 = CARTESIAN_POINT ( 'NONE',  ( 230.9489134087918671, -32.00820041275123629, 97.77040367152254419 ) ) ;
#10315 = DIRECTION ( 'NONE',  ( 1.000000000000000000, 0.000000000000000000, 0.000000000000000000 ) ) ;
#10316 = CARTESIAN_POINT ( 'NONE',  ( -85.40000000000000568, -31.30856250001229668, 101.7320508075688679 ) ) ;
#10317 = DIRECTION ( 'NONE',  ( -1.000000000000000000, -0.000000000000000000, -0.000000000000000000 ) ) ;
#10318 = CARTESIAN_POINT ( 'NONE',  ( -85.15643035625001289, -31.04062499938548569, 99.99999999999998579 ) ) ;
#10319 = CARTESIAN_POINT ( 'NONE',  ( -81.59615242270662350, -32.83259618943233704, 96.99999999999998579 ) ) ;
#10320 = CARTESIAN_POINT ( 'NONE',  ( 81.02178482187500208, -31.75312499938548427, 102.3871387122750889 ) ) ;
#10321 = ADVANCED_FACE ( 'NONE', ( #15985 ), #17644, .F. ) ;
#10322 = CARTESIAN_POINT ( 'NONE',  ( -83.90000000000000568, -32.77499999999999858, 97.40192378864668399 ) ) ;
#10323 = DIRECTION ( 'NONE',  ( 1.000000000000000000, 0.000000000000000000, -0.000000000000000000 ) ) ;
#10324 = CARTESIAN_POINT ( 'NONE',  ( -85.15643035625001289, -32.46562499938548996, 101.5914258081833879 ) ) ;
#10325 = CARTESIAN_POINT ( 'NONE',  ( -85.15643035624999868, -31.56562499938548427, -98.40857419181659793 ) ) ;
#10326 = VERTEX_POINT ( 'NONE', #19310 ) ;
#10327 = CARTESIAN_POINT ( 'NONE',  ( 80.90000000000000568, -34.14374999877097139, 102.5980762113533018 ) ) ;
#10328 = DIRECTION ( 'NONE',  ( 0.000000000000000000, -3.491481338843133355E-15, -1.000000000000000000 ) ) ;
#10329 = CARTESIAN_POINT ( 'NONE',  ( -83.77821517812500929, -32.87812499938548427, 102.3871387122750889 ) ) ;
#10330 = CARTESIAN_POINT ( 'NONE',  ( 232.5999999999999659, -32.81249999999999289, 97.00000000000000000 ) ) ;
#10331 = ORIENTED_EDGE ( 'NONE', *, *, #12234, .F. ) ;
#10332 = CARTESIAN_POINT ( 'NONE',  ( -82.39999999999999147, -33.85312499938547859, -103.1828516163667899 ) ) ;
#10333 = LINE ( 'NONE', #2905, #8795 ) ;
#10334 = VERTEX_POINT ( 'NONE', #16272 ) ;
#10335 = CARTESIAN_POINT ( 'NONE',  ( -83.20384757729338787, -32.10134618820330132, 102.9999999999999858 ) ) ;
#10336 = CARTESIAN_POINT ( 'NONE',  ( -79.64356964375001269, -33.59062499938548285, -101.5914258081833879 ) ) ;
#10337 = CARTESIAN_POINT ( 'NONE',  ( -82.39999999999999147, -32.53124999877096712, -96.53589838486223584 ) ) ;
#10338 = CARTESIAN_POINT ( 'NONE',  ( 233.9782151781249411, -32.80312499938548143, 102.3871387122750889 ) ) ;
#10339 = CARTESIAN_POINT ( 'NONE',  ( -79.39999999999999147, -32.42268749875867684, 99.99999999999998579 ) ) ;
#10340 = CARTESIAN_POINT ( 'NONE',  ( -81.02178482187500208, -34.60312499938549280, 102.3871387122750889 ) ) ;
#10341 = CARTESIAN_POINT ( 'NONE',  ( -81.02178482187500208, -34.79062499938548569, -102.3871387122750889 ) ) ;
#10342 = CARTESIAN_POINT ( 'NONE',  ( 4.000000000000000000, 2.309401076758497151, -3.433295621305379353 ) ) ;
#10343 = CARTESIAN_POINT ( 'NONE',  ( 96.99999999999994316, -21.80000000000003268, -139.9999999999999716 ) ) ;
#10344 = CARTESIAN_POINT ( 'NONE',  ( 79.39999999999999147, -32.00624999877096855, -101.7320508075688537 ) ) ;
#10345 = CARTESIAN_POINT ( 'NONE',  ( 235.5999999999999943, -33.78749999999999432, 98.26794919243110371 ) ) ;
#10346 = VERTEX_POINT ( 'NONE', #5543 ) ;
#10347 = LINE ( 'NONE', #2922, #10993 ) ;
#10348 = EDGE_CURVE ( 'NONE', #13073, #6638, #825, .T. ) ;
#10349 = CARTESIAN_POINT ( 'NONE',  ( 231.0999999999999375, -35.26874999877096428, 102.5980762113533018 ) ) ;
#10350 = CARTESIAN_POINT ( 'NONE',  ( 231.0999999999999375, -33.91874999877096286, -47.40192378864679768 ) ) ;
#10351 = CARTESIAN_POINT ( 'NONE',  ( -83.77821517812500929, -33.66562499938548569, 102.3871387122750889 ) ) ;
#10352 = EDGE_LOOP ( 'NONE', ( #10498, #18080, #15259, #9616 ) ) ;
#10353 = ORIENTED_EDGE ( 'NONE', *, *, #12952, .F. ) ;
#10354 = CARTESIAN_POINT ( 'NONE',  ( 80.90000000000000568, -34.20000000000000284, -97.40192378864668399 ) ) ;
#10355 = CARTESIAN_POINT ( 'NONE',  ( 105.1999999999999744, -34.99999999999999289, 150.0000000000000000 ) ) ;
#10356 = CARTESIAN_POINT ( 'NONE',  ( 232.5999999999999375, -29.99999999999999645, 99.99999999999998579 ) ) ;
#10357 = VERTEX_POINT ( 'NONE', #1232 ) ;
#10358 = DIRECTION ( 'NONE',  ( -1.000000000000000000, 0.000000000000000000, 0.000000000000000000 ) ) ;
#10359 = LINE ( 'NONE', #210, #18915 ) ;
#10360 = VECTOR ( 'NONE', #6711, 1000.000000000000000 ) ;
#10361 = CIRCLE ( 'NONE', #4129, 5.384454397937118664 ) ;
#10362 = CARTESIAN_POINT ( 'NONE',  ( -85.15643035625001289, -32.95312499938548711, 99.99999999999998579 ) ) ;
#10363 = CARTESIAN_POINT ( 'NONE',  ( -83.90000000000000568, -32.77499999999999858, 97.40192378864668399 ) ) ;
#10364 = CARTESIAN_POINT ( 'NONE',  ( -83.90000000000000568, -32.11874999877097281, 102.5980762113533018 ) ) ;
#10365 = DIRECTION ( 'NONE',  ( 0.000000000000000000, 0.000000000000000000, -1.000000000000000000 ) ) ;
#10366 = CARTESIAN_POINT ( 'NONE',  ( -82.40000000000000568, -30.00000000000000355, 99.99999999999998579 ) ) ;
#10367 = CARTESIAN_POINT ( 'NONE',  ( -79.69416654173919312, -35.00000000000002132, -99.37250936986646366 ) ) ;
#10368 = CARTESIAN_POINT ( 'NONE',  ( 233.9782151781249411, -30.74062499938547788, 97.61286128772489690 ) ) ;
#10369 = ORIENTED_EDGE ( 'NONE', *, *, #8001, .T. ) ;
#10370 =( NAMED_UNIT ( * ) SI_UNIT ( $, .STERADIAN. ) SOLID_ANGLE_UNIT ( ) );
#10371 = CARTESIAN_POINT ( 'NONE',  ( -85.15643035624999868, -32.80312499938548854, -98.40857419181659793 ) ) ;
#10372 = CARTESIAN_POINT ( 'NONE',  ( -0.1410422978106123659, 4.700232962125094893, -3.687027686973624707 ) ) ;
#10373 = MECHANICAL_DESIGN_GEOMETRIC_PRESENTATION_REPRESENTATION (  '', ( #18805 ), #17871 ) ;
#10374 =( BOUNDED_CURVE ( )  B_SPLINE_CURVE ( 2, ( #18785, #17219, #3542, #8234, #6577, #2463, #13990, #5314, #12622 ),
 .UNSPECIFIED., .F., .F. ) 
 B_SPLINE_CURVE_WITH_KNOTS ( ( 3, 2, 2, 2, 3 ),
 ( 0.6041666666666666297, 0.6111111111111111605, 0.6250000000000000000, 0.6388888888888888395, 0.6458333333333332593 ),
 .UNSPECIFIED. ) 
 CURVE ( )  GEOMETRIC_REPRESENTATION_ITEM ( )  RATIONAL_B_SPLINE_CURVE ( ( 0.9330127018922192983, 0.9330127018922187432, 1.000000000000000000, 0.8660254037844387076, 1.000000000000000000, 0.8660254037844387076, 1.000000000000000000, 0.9330127018922198534, 0.9330127018922192983 ) ) 
 REPRESENTATION_ITEM ( '' )  );
#10375 = CIRCLE ( 'NONE', #16308, 5.000000000000000000 ) ;
#10376 = CARTESIAN_POINT ( 'NONE',  ( 232.5999999999999375, -34.78124999877096002, -47.00000000000011369 ) ) ;
#10377 = CARTESIAN_POINT ( 'NONE',  ( -79.64356964375001269, -31.30312499938548854, 101.5914258081833879 ) ) ;
#10378 = DIRECTION ( 'NONE',  ( 0.000000000000000000, 0.000000000000000000, 1.000000000000000000 ) ) ;
#10379 = CARTESIAN_POINT ( 'NONE',  ( 231.2217848218749339, -32.31562499938547717, -47.61286128772501769 ) ) ;
#10380 = ORIENTED_EDGE ( 'NONE', *, *, #11281, .T. ) ;
#10381 = EDGE_LOOP ( 'NONE', ( #3281, #12253, #8885, #3407 ) ) ;
#10382 = CARTESIAN_POINT ( 'NONE',  ( -84.67508262029694777, -32.00000000000000711, 101.5663513044662665 ) ) ;
#10383 = CARTESIAN_POINT ( 'NONE',  ( -79.39999999999999147, -31.16250000000000497, 101.7320508075688537 ) ) ;
#10384 = CARTESIAN_POINT ( 'NONE',  ( -79.39999999999999147, -31.96874999877096712, 99.99999999999998579 ) ) ;
#10385 = CARTESIAN_POINT ( 'NONE',  ( 85.40000000000000568, -33.14999999999999858, 99.99999999999998579 ) ) ;
#10386 = CARTESIAN_POINT ( 'NONE',  ( -94.79999999999999716, 0.000000000000000000, 150.0000000000000000 ) ) ;
#10388 = CARTESIAN_POINT ( 'NONE',  ( 231.2217848218749339, -34.11562499938548143, 102.3871387122750889 ) ) ;
#10387 = AXIS2_PLACEMENT_3D ( 'NONE', #575, #8179, #672 ) ;
#10389 = CARTESIAN_POINT ( 'NONE',  ( 235.3564303562499447, -34.82812499938548001, -51.59142580818350154 ) ) ;
#10390 = CARTESIAN_POINT ( 'NONE',  ( 79.64356964374999848, -33.96562499938548285, 99.99999999999998579 ) ) ;
#10391 = CARTESIAN_POINT ( 'NONE',  ( 85.15643035624999868, -31.45312499938548356, -101.5914258081833879 ) ) ;
#10392 = ORIENTED_EDGE ( 'NONE', *, *, #18134, .T. ) ;
#10393 = CARTESIAN_POINT ( 'NONE',  ( 229.8435696437499303, -34.64062499938548001, -50.00000000000011369 ) ) ;
#10394 = CARTESIAN_POINT ( 'NONE',  ( 79.39999999999999147, -34.21874999877096712, 99.99999999999998579 ) ) ;
#10395 = CARTESIAN_POINT ( 'NONE',  ( 83.77821517812500929, -34.11562499938548854, -102.3871387122750889 ) ) ;
#10396 = ORIENTED_EDGE ( 'NONE', *, *, #3306, .T. ) ;
#10397 = DIRECTION ( 'NONE',  ( 2.312964634635740689E-14, 0.000000000000000000, -1.000000000000000000 ) ) ;
#10398 = CARTESIAN_POINT ( 'NONE',  ( -82.40000000000000568, -34.55624999877097281, 97.00000000000000000 ) ) ;
#10399 = CARTESIAN_POINT ( 'NONE',  ( 233.9782151781249411, -30.85312499938547859, -52.38713871227520968 ) ) ;
#10400 = CARTESIAN_POINT ( 'NONE',  ( -85.15643035624999868, -35.11426541925033007, 98.99674735228809652 ) ) ;
#10401 = VERTEX_POINT ( 'NONE', #4352 ) ;
#10402 = CARTESIAN_POINT ( 'NONE',  ( -85.40000000000000568, -33.95624999877097139, 101.7320508075688821 ) ) ;
#10403 = CARTESIAN_POINT ( 'NONE',  ( 231.2217848218749339, -34.56562499938547717, 102.3871387122750889 ) ) ;
#10404 = CARTESIAN_POINT ( 'NONE',  ( 0.000000000000000000, 0.000000000000000000, 0.000000000000000000 ) ) ;
#10405 = CARTESIAN_POINT ( 'NONE',  ( -83.90000000000000568, -31.42106250001229384, 97.40192378864668399 ) ) ;
#10406 = DIRECTION ( 'NONE',  ( -0.000000000000000000, 1.000000000000000000, 0.000000000000000000 ) ) ;
#10407 = CARTESIAN_POINT ( 'NONE',  ( -79.68596062386968981, -32.00000000000002132, 101.2782762865727619 ) ) ;
#10408 = CARTESIAN_POINT ( 'NONE',  ( -79.64356964375001269, -31.30312499938548854, 101.5914258081833879 ) ) ;
#10409 = CARTESIAN_POINT ( 'NONE',  ( -81.59615242270662350, -32.38259618943233420, 96.99999999999998579 ) ) ;
#10410 = CARTESIAN_POINT ( 'NONE',  ( 83.77821517812500929, -32.42812499938548854, 97.61286128772489690 ) ) ;
#10411 = LINE ( 'NONE', #7667, #9276 ) ;
#10412 = CARTESIAN_POINT ( 'NONE',  ( -82.40000000000000568, -30.00000000000000355, 99.99999999999998579 ) ) ;
#10413 = CYLINDRICAL_SURFACE ( 'NONE', #6953, 3.000000000000002665 ) ;
#10414 = CARTESIAN_POINT ( 'NONE',  ( -79.64356964375001269, -32.24062499938548854, -101.5914258081833879 ) ) ;
#10415 = ORIENTED_EDGE ( 'NONE', *, *, #3294, .F. ) ;
#10416 = CARTESIAN_POINT ( 'NONE',  ( 85.15643035624999868, -31.19062499938548783, 101.5914258081833879 ) ) ;
#10417 = DIRECTION ( 'NONE',  ( 1.000000000000000000, 0.000000000000000000, 0.000000000000000000 ) ) ;
#10418 = DIRECTION ( 'NONE',  ( 1.000000000000000000, 0.000000000000000000, -0.000000000000000000 ) ) ;
#10419 = CARTESIAN_POINT ( 'NONE',  ( 4.175813232069148562, -2.061359961916374495, -3.570380186727398097 ) ) ;
#10420 = CARTESIAN_POINT ( 'NONE',  ( -79.64356964374999848, -31.37812499938548427, 99.99999999999998579 ) ) ;
#10421 = DIRECTION ( 'NONE',  ( 0.000000000000000000, 0.000000000000000000, 1.000000000000000000 ) ) ;
#10422 = ORIENTED_EDGE ( 'NONE', *, *, #925, .T. ) ;
#10423 = CARTESIAN_POINT ( 'NONE',  ( -85.40000000000000568, -31.35000000000000142, -99.99999999999998579 ) ) ;
#10424 = CARTESIAN_POINT ( 'NONE',  ( 4.000000000000000000, -2.471525695159793035, -3.686886880705770864 ) ) ;
#10425 = EDGE_CURVE ( 'NONE', #13758, #12372, #4067, .T. ) ;
#10426 = CARTESIAN_POINT ( 'NONE',  ( -82.39999999999999147, -33.51562499938548001, -103.1828516163667899 ) ) ;
#10427 = DIRECTION ( 'NONE',  ( 0.000000000000000000, 0.000000000000000000, -1.000000000000000000 ) ) ;
#10428 = CARTESIAN_POINT ( 'NONE',  ( -79.39999999999999147, -32.00624999877096855, -98.26794919243113213 ) ) ;
#10429 = CARTESIAN_POINT ( 'NONE',  ( 235.3564303562499447, -30.96562499938547930, 101.5914258081833879 ) ) ;
#10430 = CARTESIAN_POINT ( 'NONE',  ( -80.90000000000000568, -30.69768749875868252, 102.5980762113533018 ) ) ;
#10431 = CARTESIAN_POINT ( 'NONE',  ( -82.39999999999999147, -32.84062499938548996, 103.1828516163667899 ) ) ;
#10432 = FACE_OUTER_BOUND ( 'NONE', #14313, .T. ) ;
#10433 = CARTESIAN_POINT ( 'NONE',  ( 85.15643035625001289, -32.87812499938548427, 101.5914258081833879 ) ) ;
#10434 = DIRECTION ( 'NONE',  ( 1.000000000000000000, 0.000000000000000000, -0.000000000000000000 ) ) ;
#10435 = DIRECTION ( 'NONE',  ( 1.000000000000000000, -0.000000000000000000, -2.407412430484046130E-31 ) ) ;
#10436 = CARTESIAN_POINT ( 'NONE',  ( 85.40000000000000568, -34.40624999877096712, -101.7320508075688679 ) ) ;
#10437 = CARTESIAN_POINT ( 'NONE',  ( 229.5999999999999375, -34.08749999999999147, 98.26794919243111792 ) ) ;
#10438 = ADVANCED_FACE ( 'NONE', ( #16368 ), #8453, .T. ) ;
#10439 = ORIENTED_EDGE ( 'NONE', *, *, #18544, .F. ) ;
#10440 = CARTESIAN_POINT ( 'NONE',  ( 232.5999999999999943, -33.74062499938548143, -46.81714838363331666 ) ) ;
#10441 = DIRECTION ( 'NONE',  ( 4.814824860968092260E-31, -1.336382355046098552E-47, 1.000000000000000000 ) ) ;
#10442 = CARTESIAN_POINT ( 'NONE',  ( 232.5999999999999375, -34.33124999877096428, 103.4641016151377499 ) ) ;
#10443 = CARTESIAN_POINT ( 'NONE',  ( 232.5999999999999375, -34.10624999877096286, -53.46410161513786363 ) ) ;
#10444 = ADVANCED_FACE ( 'NONE', ( #10216 ), #11678, .F. ) ;
#10445 = CARTESIAN_POINT ( 'NONE',  ( -82.39999999999999147, -33.17812499938548854, 103.1828516163667899 ) ) ;
#10446 = ORIENTED_EDGE ( 'NONE', *, *, #14324, .T. ) ;
#10447 = VERTEX_POINT ( 'NONE', #16181 ) ;
#10448 = DIRECTION ( 'NONE',  ( 1.000000000000000000, 0.000000000000000000, -0.000000000000000000 ) ) ;
#10449 = CARTESIAN_POINT ( 'NONE',  ( -3.999999999998910649, -1.658469974638591804, -3.531532913075256186 ) ) ;
#10450 = CARTESIAN_POINT ( 'NONE',  ( 4.175572532730935649, -4.122058607836119215, -1.475653861719983332E-15 ) ) ;
#10451 = ORIENTED_EDGE ( 'NONE', *, *, #15263, .F. ) ;
#10452 = CARTESIAN_POINT ( 'NONE',  ( 81.59615242270663771, -32.51115380933863008, -103.0000000000000000 ) ) ;
#10453 = DIRECTION ( 'NONE',  ( -0.000000000000000000, -0.000000000000000000, -1.000000000000000000 ) ) ;
#10454 = PRESENTATION_LAYER_ASSIGNMENT (  '', '', ( #806 ) ) ;
#10455 = CARTESIAN_POINT ( 'NONE',  ( -83.77821517812500929, -33.47812499938548569, 97.61286128772489690 ) ) ;
#10456 = CARTESIAN_POINT ( 'NONE',  ( -85.40000000000000568, -34.01250000000000284, 101.7320508075688679 ) ) ;
#10457 = EDGE_CURVE ( 'NONE', #5172, #6865, #2791, .T. ) ;
#10458 = CARTESIAN_POINT ( 'NONE',  ( -80.90000000000000568, -32.04374999877096997, 102.5980762113533018 ) ) ;
#10459 = CARTESIAN_POINT ( 'NONE',  ( 0.000000000000000000, 0.000000000000000000, 0.000000000000000000 ) ) ;
#10460 =( NAMED_UNIT ( * ) SI_UNIT ( $, .STERADIAN. ) SOLID_ANGLE_UNIT ( ) );
#10461 = CARTESIAN_POINT ( 'NONE',  ( 110.0000000000000142, 15.19999999999995310, 50.00000000000001421 ) ) ;
#10462 = DIRECTION ( 'NONE',  ( -1.000000000000000000, 0.000000000000000000, 0.000000000000000000 ) ) ;
#10463 = ORIENTED_EDGE ( 'NONE', *, *, #18600, .T. ) ;
#10464 = CARTESIAN_POINT ( 'NONE',  ( -85.15643035625001289, -32.84062499938548285, -99.99999999999998579 ) ) ;
#10465 = CARTESIAN_POINT ( 'NONE',  ( 3.540020015735602765, 2.810662092924382627, -3.602146406945867962 ) ) ;
#10466 = CONICAL_SURFACE ( 'NONE', #5804, 2.059999999999998721, 0.9599310885968738161 ) ;
#10467 = CARTESIAN_POINT ( 'NONE',  ( -82.39999999999999147, -31.40624999877096712, 96.99999999999998579 ) ) ;
#10468 = CARTESIAN_POINT ( 'NONE',  ( 80.80861089413672005, -34.99999999999999289, -102.2789443502789055 ) ) ;
#10469 = CARTESIAN_POINT ( 'NONE',  ( -79.64356964375001269, -30.77812499938548285, 98.40857419181659793 ) ) ;
#10470 = CARTESIAN_POINT ( 'NONE',  ( 82.39999999999999147, -32.36250000000000426, 102.9999999999999858 ) ) ;
#10471 = EDGE_CURVE ( 'NONE', #2762, #12007, #13049, .T. ) ;
#10472 = CARTESIAN_POINT ( 'NONE',  ( 232.5999999999999375, -32.72812499938547859, -46.81714838363331666 ) ) ;
#10473 = ORIENTED_EDGE ( 'NONE', *, *, #2775, .F. ) ;
#10474 = VERTEX_POINT ( 'NONE', #17835 ) ;
#10475 = B_SPLINE_CURVE_WITH_KNOTS ( 'NONE', 3,
 ( #16380, #2990, #18052, #9047, #8758, #15011 ),
 .UNSPECIFIED., .F., .F.,
 ( 4, 2, 4 ),
 ( 0.002365888236227977302, 0.003551327329835078910, 0.004736766423442180518 ),
 .UNSPECIFIED. ) ;
#10476 = DIRECTION ( 'NONE',  ( 0.000000000000000000, 1.000000000000000000, 0.000000000000000000 ) ) ;
#10477 = CARTESIAN_POINT ( 'NONE',  ( -79.39999999999999147, -31.12500000000000355, 99.99999999999998579 ) ) ;
#10478 = CARTESIAN_POINT ( 'NONE',  ( -79.39999999999999147, -32.86874999877097281, 99.99999999999998579 ) ) ;
#10479 = CARTESIAN_POINT ( 'NONE',  ( 79.39999999999999147, -32.02500000000000568, 99.99999999999998579 ) ) ;
#10480 = ADVANCED_FACE ( 'NONE', ( #13333 ), #14695, .F. ) ;
#10481 = CARTESIAN_POINT ( 'NONE',  ( 5.100000000000002309, 6.368163355566238354E-16, -5.200000000000001066 ) ) ;
#10482 = CARTESIAN_POINT ( 'NONE',  ( 235.3564303562499447, -34.37812499938547717, 98.40857419181659793 ) ) ;
#10483 = AXIS2_PLACEMENT_3D ( 'NONE', #4672, #13456, #10427 ) ;
#10484 = CARTESIAN_POINT ( 'NONE',  ( 232.5999999999999943, -33.17812499938548143, -46.81714838363331666 ) ) ;
#10485 = CARTESIAN_POINT ( 'NONE',  ( 82.61711639270117757, -31.99999999999999289, -97.16008101252806739 ) ) ;
#10486 =( BOUNDED_CURVE ( )  B_SPLINE_CURVE ( 2, ( #12820, #17027, #14086, #15465, #2177, #15856, #3824, #17318, #2076 ),
 .UNSPECIFIED., .F., .F. ) 
 B_SPLINE_CURVE_WITH_KNOTS ( ( 3, 2, 2, 2, 3 ),
 ( 0.6875000000000000000, 0.6944444444444444198, 0.7083333333333333703, 0.7222222222222222099, 0.7291666666666668517 ),
 .UNSPECIFIED. ) 
 CURVE ( )  GEOMETRIC_REPRESENTATION_ITEM ( )  RATIONAL_B_SPLINE_CURVE ( ( 0.9330127018922194093, 0.9330127018922194093, 1.000000000000000000, 0.8660254037844387076, 1.000000000000000000, 0.8660254037844387076, 1.000000000000000000, 0.9330127018922177440, 0.9330127018922194093 ) ) 
 REPRESENTATION_ITEM ( '' )  );
#10487 = CARTESIAN_POINT ( 'NONE',  ( 82.39999999999999147, -30.70312499938548711, -96.81714838363319586 ) ) ;
#10488 = ORIENTED_EDGE ( 'NONE', *, *, #1235, .T. ) ;
#10489 = CARTESIAN_POINT ( 'NONE',  ( 229.5999999999999375, -29.99999999999999645, -50.00000000000011369 ) ) ;
#10490 = CARTESIAN_POINT ( 'NONE',  ( 80.90000000000000568, -34.14374999877097139, 102.5980762113533018 ) ) ;
#10491 = CARTESIAN_POINT ( 'NONE',  ( 82.39999999999999147, -33.85312499938547859, -96.81714838363319586 ) ) ;
#10492 = AXIS2_PLACEMENT_3D ( 'NONE', #16600, #17974, #4584 ) ;
#10493 = FACE_OUTER_BOUND ( 'NONE', #8359, .T. ) ;
#10494 = CARTESIAN_POINT ( 'NONE',  ( -82.40000000000000568, -30.00000000000000355, 96.99999999999998579 ) ) ;
#10495 = CARTESIAN_POINT ( 'NONE',  ( 235.3564303562499447, -30.47812499938547859, -50.00000000000011369 ) ) ;
#10496 = VECTOR ( 'NONE', #11892, 1000.000000000000000 ) ;
#10497 = CARTESIAN_POINT ( 'NONE',  ( -82.39999999999999147, -30.33750000000000213, 103.4641016151377499 ) ) ;
#10498 = ORIENTED_EDGE ( 'NONE', *, *, #2437, .F. ) ;
#10499 = CARTESIAN_POINT ( 'NONE',  ( -80.90000000000000568, -34.35000000000000853, 102.5980762113533018 ) ) ;
#10500 = CARTESIAN_POINT ( 'NONE',  ( 82.39999999999999147, -30.25312499938548783, 103.1828516163667899 ) ) ;
#10501 = CARTESIAN_POINT ( 'NONE',  ( -85.40000000000000568, -31.75856250001229242, 101.7320508075688679 ) ) ;
#10502 = PRODUCT_DEFINITION_FORMATION_WITH_SPECIFIED_SOURCE ( 'ANY', '', #8424, .NOT_KNOWN. ) ;
#10503 = LINE ( 'NONE', #1528, #6432 ) ;
#10504 = CARTESIAN_POINT ( 'NONE',  ( 249.9999999999999716, -29.80000000000000426, -100.0000000000000000 ) ) ;
#10505 = CARTESIAN_POINT ( 'NONE',  ( -82.39999999999999147, -32.50312499938548427, 96.81714838363319586 ) ) ;
#10506 = CARTESIAN_POINT ( 'NONE',  ( 230.9316747517339081, -35.00000000000000000, 102.2567273996571515 ) ) ;
#10507 = CARTESIAN_POINT ( 'NONE',  ( 82.39999999999999147, -32.61562499938548854, 103.1828516163667899 ) ) ;
#10508 = CARTESIAN_POINT ( 'NONE',  ( 83.77821517812500929, -30.32812499938548711, -97.61286128772489690 ) ) ;
#10509 = FACE_OUTER_BOUND ( 'NONE', #5099, .T. ) ;
#10510 = CARTESIAN_POINT ( 'NONE',  ( -85.14613134194615895, -31.99999999999997868, -100.2978599400816364 ) ) ;
#10511 = CARTESIAN_POINT ( 'NONE',  ( -83.77821517812500929, -32.12812499938548427, -102.3871387122750889 ) ) ;
#10512 = ORIENTED_EDGE ( 'NONE', *, *, #10425, .T. ) ;
#10513 = CARTESIAN_POINT ( 'NONE',  ( 79.39999999999999147, -35.08124999877097139, 101.7320508075688821 ) ) ;
#10514 = AXIS2_PLACEMENT_3D ( 'NONE', #14565, #17609, #17228 ) ;
#10515 = CARTESIAN_POINT ( 'NONE',  ( 83.20384757729338787, -34.53615380933862866, 102.9999999999999858 ) ) ;
#10516 = CARTESIAN_POINT ( 'NONE',  ( 232.5999999999999375, -34.64062499938548001, -46.81714838363331666 ) ) ;
#10517 = CARTESIAN_POINT ( 'NONE',  ( -82.40000000000001990, -33.26250000000000284, 97.00000000000000000 ) ) ;
#10518 = CARTESIAN_POINT ( 'NONE',  ( -85.15643035624999868, -31.56562499938548427, 101.5914258081833879 ) ) ;
#10519 = CARTESIAN_POINT ( 'NONE',  ( 82.39999999999999147, -33.65624999877097423, -97.00000000000000000 ) ) ;
#10520 = VERTEX_POINT ( 'NONE', #10122 ) ;
#10521 = CARTESIAN_POINT ( 'NONE',  ( -80.90000000000000568, -31.05000000000000071, -102.5980762113533018 ) ) ;
#10522 = AXIS2_PLACEMENT_3D ( 'NONE', #14184, #9992, #15567 ) ;
#10523 = CARTESIAN_POINT ( 'NONE',  ( 4.033895293471413623, 1.419609371826631827, -3.499999999999999112 ) ) ;
#10524 = CARTESIAN_POINT ( 'NONE',  ( 113.0000000000000000, 5.199999999999948663, 41.33974596215564645 ) ) ;
#10525 = CARTESIAN_POINT ( 'NONE',  ( -79.64356964374999848, -33.62812499938548427, -99.99999999999998579 ) ) ;
#10526 = CARTESIAN_POINT ( 'NONE',  ( 229.5999999999999375, -34.49999999999999289, -50.00000000000011369 ) ) ;
#10527 = CARTESIAN_POINT ( 'NONE',  ( 235.3564303562499447, -31.34062499938548285, 98.40857419181659793 ) ) ;
#10528 = CARTESIAN_POINT ( 'NONE',  ( -80.90000000000000568, -31.14768749875868181, 102.5980762113533018 ) ) ;
#10529 = AXIS2_PLACEMENT_3D ( 'NONE', #11135, #6659, #3325 ) ;
#10530 = CARTESIAN_POINT ( 'NONE',  ( -85.15643035625001289, -34.75312499938548427, 99.99999999999998579 ) ) ;
#10531 = CARTESIAN_POINT ( 'NONE',  ( -79.64356964374998427, -34.90312499938548285, -98.40857419181659793 ) ) ;
#10532 = CARTESIAN_POINT ( 'NONE',  ( 79.64356964374999848, -32.61562499938548854, 99.99999999999998579 ) ) ;
#10533 = CARTESIAN_POINT ( 'NONE',  ( 81.59615242270662350, -32.56740381056766864, -103.0000000000000000 ) ) ;
#10534 =( BOUNDED_CURVE ( )  B_SPLINE_CURVE ( 2, ( #4714, #4325, #15059, #7633, #3231, #6084, #6280, #7346, #5891 ),
 .UNSPECIFIED., .F., .F. ) 
 B_SPLINE_CURVE_WITH_KNOTS ( ( 3, 2, 2, 2, 3 ),
 ( 0.3958333333333334259, 0.4027777777777777901, 0.4166666666666666852, 0.4305555555555555802, 0.4374999999999999445 ),
 .UNSPECIFIED. ) 
 CURVE ( )  GEOMETRIC_REPRESENTATION_ITEM ( )  RATIONAL_B_SPLINE_CURVE ( ( 0.9330127018922192983, 0.9330127018922200755, 1.000000000000000000, 0.8660254037844387076, 1.000000000000000000, 0.8660254037844387076, 1.000000000000000000, 0.9330127018922198534, 0.9330127018922192983 ) ) 
 REPRESENTATION_ITEM ( '' )  );
#10535 = DIRECTION ( 'NONE',  ( 0.000000000000000000, 0.000000000000000000, -1.000000000000000000 ) ) ;
#10536 = CARTESIAN_POINT ( 'NONE',  ( 79.39999999999999147, -35.08124999877097139, -98.26794919243110371 ) ) ;
#10537 = AXIS2_PLACEMENT_3D ( 'NONE', #2821, #6050, #8777 ) ;
#10538 = CARTESIAN_POINT ( 'NONE',  ( 235.5999999999999375, -34.72499999999999432, 99.99999999999998579 ) ) ;
#10539 = EDGE_CURVE ( 'NONE', #13022, #12416, #6110, .T. ) ;
#10540 = AXIS2_PLACEMENT_3D ( 'NONE', #7341, #19270, #11738 ) ;
#10541 = EDGE_CURVE ( 'NONE', #10812, #7830, #13278, .T. ) ;
#10542 = ORIENTED_EDGE ( 'NONE', *, *, #13895, .F. ) ;
#10543 = CARTESIAN_POINT ( 'NONE',  ( 232.5999999999999943, -33.51562499938548001, -53.18285161636690361 ) ) ;
#10544 = DIRECTION ( 'NONE',  ( 1.000000000000000000, 0.000000000000000000, 0.000000000000000000 ) ) ;
#10545 = CARTESIAN_POINT ( 'NONE',  ( 229.8435696437499871, -31.11562499938547788, 101.5914258081833879 ) ) ;
#10546 = CARTESIAN_POINT ( 'NONE',  ( 235.5999999999999943, -32.45624999877096428, -48.26794919243124582 ) ) ;
#10547 = CARTESIAN_POINT ( 'NONE',  ( -79.64356964374998427, -33.02812499938548285, 98.40857419181659793 ) ) ;
#10548 = ORIENTED_EDGE ( 'NONE', *, *, #4234, .F. ) ;
#10549 = ORIENTED_EDGE ( 'NONE', *, *, #5654, .F. ) ;
#10550 = CARTESIAN_POINT ( 'NONE',  ( 4.114405500665267112, 2.025575754679705298, -3.508400121684926987 ) ) ;
#10551 = PLANE ( 'NONE',  #4128 ) ;
#10552 = CARTESIAN_POINT ( 'NONE',  ( -83.20384757729335945, -33.69240381056766154, -102.9999999999999858 ) ) ;
#10553 = ORIENTED_EDGE ( 'NONE', *, *, #315, .F. ) ;
#10554 = CARTESIAN_POINT ( 'NONE',  ( -82.40000000000000568, -31.63124999877096855, 102.9999999999999858 ) ) ;
#10555 = CARTESIAN_POINT ( 'NONE',  ( 232.5999999999999659, -32.58749999999999858, 102.9999999999999858 ) ) ;
#10556 = AXIS2_PLACEMENT_3D ( 'NONE', #7528, #4505, #6173 ) ;
#10557 = EDGE_CURVE ( 'NONE', #4900, #1498, #12950, .T. ) ;
#10558 = CARTESIAN_POINT ( 'NONE',  ( -82.39999999999999147, -33.06562499938548427, 96.81714838363319586 ) ) ;
#10559 = CARTESIAN_POINT ( 'NONE',  ( -84.69814161231455785, -35.00052329606839407, 98.07164704222793716 ) ) ;
#10560 = CARTESIAN_POINT ( 'NONE',  ( -85.40000000000000568, -32.23124999877096997, 98.26794919243111792 ) ) ;
#10561 = LINE ( 'NONE', #1763, #3799 ) ;
#10562 = CARTESIAN_POINT ( 'NONE',  ( 3.950241966888465406, 2.668221755853712907, 2.378504353001160254 ) ) ;
#10563 = CARTESIAN_POINT ( 'NONE',  ( -82.40000000000000568, -30.00000000000000355, 99.99999999999998579 ) ) ;
#10564 = EDGE_CURVE ( 'NONE', #12925, #2988, #194, .T. ) ;
#10565 = CARTESIAN_POINT ( 'NONE',  ( 232.5999999999999375, -31.37812499938547717, 103.1828516163667899 ) ) ;
#10566 = ORIENTED_EDGE ( 'NONE', *, *, #3342, .T. ) ;
#10567 = CARTESIAN_POINT ( 'NONE',  ( -85.15643035624999868, -33.25312499938548427, -98.40857419181659793 ) ) ;
#10568 = LINE ( 'NONE', #1679, #15838 ) ;
#10569 = VECTOR ( 'NONE', #2409, 1000.000000000000000 ) ;
#10570 = CARTESIAN_POINT ( 'NONE',  ( 235.5999999999999943, -33.78750000000000142, 98.26794919243110371 ) ) ;
#10571 = DIRECTION ( 'NONE',  ( 0.000000000000000000, 1.000000000000000000, 0.000000000000000000 ) ) ;
#10572 = CARTESIAN_POINT ( 'NONE',  ( -79.64356964374999848, -30.36562499938548498, 99.99999999999998579 ) ) ;
#10573 = DIRECTION ( 'NONE',  ( 0.000000000000000000, -1.000000000000000000, 0.000000000000000000 ) ) ;
#10574 = CARTESIAN_POINT ( 'NONE',  ( 235.3564303562499447, -34.90312499938547575, -48.40857419181671162 ) ) ;
#10575 = ORIENTED_EDGE ( 'NONE', *, *, #10788, .F. ) ;
#10576 = VERTEX_POINT ( 'NONE', #13811 ) ;
#10577 = CARTESIAN_POINT ( 'NONE',  ( -85.40000000000000568, -31.80000000000000071, 99.99999999999998579 ) ) ;
#10578 = CARTESIAN_POINT ( 'NONE',  ( -85.40000000000000568, -30.03750000000000497, 98.26794919243111792 ) ) ;
#10579 = CARTESIAN_POINT ( 'NONE',  ( -85.40000000000000568, -31.33124999877096428, 98.26794919243111792 ) ) ;
#10581 = CARTESIAN_POINT ( 'NONE',  ( 80.90000000000000568, -32.55000000000000426, 97.40192378864668399 ) ) ;
#10580 =( REPRESENTATION_RELATIONSHIP ('NONE','NONE', #14468, #19222 ) REPRESENTATION_RELATIONSHIP_WITH_TRANSFORMATION ( #8563 )SHAPE_REPRESENTATION_RELATIONSHIP( ) );
#10582 = CARTESIAN_POINT ( 'NONE',  ( -80.24533121543035463, -32.00000000000000711, -97.95829548583749613 ) ) ;
#10583 = CARTESIAN_POINT ( 'NONE',  ( 232.5999999999999375, -33.17812499938548143, 103.1828516163667899 ) ) ;
#10584 = CARTESIAN_POINT ( 'NONE',  ( 235.3564303562499447, -33.55312499938548143, -48.40857419181671162 ) ) ;
#10585 = DIRECTION ( 'NONE',  ( 0.000000000000000000, 0.000000000000000000, 1.000000000000000000 ) ) ;
#10586 = CARTESIAN_POINT ( 'NONE',  ( 81.02178482187500208, -32.24062499938548854, -102.3871387122750889 ) ) ;
#10587 = VERTEX_POINT ( 'NONE', #3073 ) ;
#10588 = CARTESIAN_POINT ( 'NONE',  ( 229.5999999999999375, -31.76249999999999218, -48.26794919243123161 ) ) ;
#10589 = CARTESIAN_POINT ( 'NONE',  ( 83.20384757729335945, -34.85759618943233562, -102.9999999999999716 ) ) ;
#10590 = CARTESIAN_POINT ( 'NONE',  ( 81.02178482187500208, -33.44062499938548427, -97.61286128772489690 ) ) ;
#10591 = DIRECTION ( 'NONE',  ( 0.000000000000000000, 0.000000000000000000, -1.000000000000000000 ) ) ;
#10592 = DIRECTION ( 'NONE',  ( 1.000000000000000000, -0.000000000000000000, -2.407412430484046130E-31 ) ) ;
#10593 = EDGE_CURVE ( 'NONE', #15647, #18009, #13432, .T. ) ;
#10594 = CARTESIAN_POINT ( 'NONE',  ( 233.9782151781249411, -31.45312499938548356, -47.61286128772501769 ) ) ;
#10595 = CARTESIAN_POINT ( 'NONE',  ( -85.15643035624999868, -34.67812499938548143, 98.40857419181659793 ) ) ;
#10596 = ORIENTED_EDGE ( 'NONE', *, *, #9611, .F. ) ;
#10597 = CARTESIAN_POINT ( 'NONE',  ( -83.81335597582008745, -34.99989732956152721, 102.6513159617165201 ) ) ;
#10598 = CARTESIAN_POINT ( 'NONE',  ( 235.3564303562499447, -34.45312499938548001, 101.5914258081833879 ) ) ;
#10599 = CARTESIAN_POINT ( 'NONE',  ( 83.77821517812500929, -30.96562499938548640, 97.61286128772489690 ) ) ;
#10600 = CARTESIAN_POINT ( 'NONE',  ( -85.40000000000000568, -33.18356250001228602, 98.26794919243111792 ) ) ;
#10601 =( BOUNDED_CURVE ( )  B_SPLINE_CURVE ( 2, ( #7965, #750, #1813, #6705, #12650, #15294, #9233, #15196, #16763 ),
 .UNSPECIFIED., .F., .F. ) 
 B_SPLINE_CURVE_WITH_KNOTS ( ( 3, 2, 2, 2, 3 ),
 ( 0.4791666666666666297, 0.4861111111111111049, 0.5000000000000000000, 0.5138888888888888395, 0.5208333333333333703 ),
 .UNSPECIFIED. ) 
 CURVE ( )  GEOMETRIC_REPRESENTATION_ITEM ( )  RATIONAL_B_SPLINE_CURVE ( ( 0.9330127018922194093, 0.9330127018922190762, 1.000000000000000000, 0.8660254037844387076, 1.000000000000000000, 0.8660254037844387076, 1.000000000000000000, 0.9330127018922187432, 0.9330127018922192983 ) ) 
 REPRESENTATION_ITEM ( '' )  );
#10602 = B_SPLINE_CURVE_WITH_KNOTS ( 'NONE', 3,
 ( #1400, #140, #7353, #16440, #1308, #6090 ),
 .UNSPECIFIED., .F., .F.,
 ( 4, 2, 4 ),
 ( 0.002044882221487541018, 0.003063384235218501520, 0.004081886248949461587 ),
 .UNSPECIFIED. ) ;
#10603 = CARTESIAN_POINT ( 'NONE',  ( -83.20384757729335945, -33.24240381056766580, -102.9999999999999716 ) ) ;
#10604 = CARTESIAN_POINT ( 'NONE',  ( -80.90000000000000568, -32.40000000000000568, 97.40192378864668399 ) ) ;
#10605 = CARTESIAN_POINT ( 'NONE',  ( 85.15643035624999868, -30.62812499938548427, 101.5914258081833879 ) ) ;
#10606 = CARTESIAN_POINT ( 'NONE',  ( 80.08630547029510183, -32.02340763552835057, 97.87171054440995022 ) ) ;
#10607 = CARTESIAN_POINT ( 'NONE',  ( -79.39999999999999147, -32.47500000000000142, -99.99999999999998579 ) ) ;
#10608 = CARTESIAN_POINT ( 'NONE',  ( -94.79999999999999716, -35.00000000000000000, -150.0000000000000000 ) ) ;
#10609 = CARTESIAN_POINT ( 'NONE',  ( -82.39999999999999147, -30.59062499938548640, -96.81714838363319586 ) ) ;
#10610 = EDGE_LOOP ( 'NONE', ( #12833, #17979, #2734, #1912, #7797, #10189, #18983, #5373, #6619, #7063, #17105, #6921, #17184, #7220, #14358, #9920, #4205 ) ) ;
#10611 = CARTESIAN_POINT ( 'NONE',  ( 81.02178482187500208, -30.40312499938548640, 102.3871387122750889 ) ) ;
#10612 = DIRECTION ( 'NONE',  ( 0.000000000000000000, 0.000000000000000000, 1.000000000000000000 ) ) ;
#10613 = LINE ( 'NONE', #7778, #3655 ) ;
#10614 = CARTESIAN_POINT ( 'NONE',  ( -79.64356964374999848, -32.27812499938548996, 99.99999999999998579 ) ) ;
#10615 = CARTESIAN_POINT ( 'NONE',  ( 85.40000000000000568, -33.09374999877096712, 99.99999999999998579 ) ) ;
#10616 = ORIENTED_EDGE ( 'NONE', *, *, #17770, .F. ) ;
#10617 = CARTESIAN_POINT ( 'NONE',  ( -80.90000000000000568, -31.94999999999999929, -102.5980762113533018 ) ) ;
#10618 = CARTESIAN_POINT ( 'NONE',  ( 82.85024983566745505, -34.99999999999999289, 102.9730910282409440 ) ) ;
#10619 = CARTESIAN_POINT ( 'NONE',  ( 83.90000000000000568, -34.96874999877096712, -97.40192378864668399 ) ) ;
#10620 = CARTESIAN_POINT ( 'NONE',  ( -85.15643035625001289, -33.40312499938548285, -99.99999999999998579 ) ) ;
#10621 = CARTESIAN_POINT ( 'NONE',  ( 94.79999999999995453, -5.200000000000000178, -150.0000000000000000 ) ) ;
#10622 = CARTESIAN_POINT ( 'NONE',  ( 229.8435696437499871, -32.09062499938548285, 98.40857419181659793 ) ) ;
#10623 = CARTESIAN_POINT ( 'NONE',  ( -82.39999999999999147, -30.73518749875867684, 103.4641016151377499 ) ) ;
#10624 = ADVANCED_FACE ( 'NONE', ( #9318, #6306 ), #18128, .T. ) ;
#10625 = CARTESIAN_POINT ( 'NONE',  ( -85.15643035624999868, -32.46562499938548996, 101.5914258081833879 ) ) ;
#10626 = CARTESIAN_POINT ( 'NONE',  ( -79.64356964374999848, -33.96562499938548285, -99.99999999999998579 ) ) ;
#10627 = CARTESIAN_POINT ( 'NONE',  ( 81.02178482187500208, -33.89062499938548711, 102.3871387122750889 ) ) ;
#10628 = DIRECTION ( 'NONE',  ( -1.000000000000000000, 0.000000000000000000, -0.000000000000000000 ) ) ;
#10629 = CARTESIAN_POINT ( 'NONE',  ( 85.40000000000000568, -32.66250000000000142, -101.7320508075688821 ) ) ;
#10630 = CARTESIAN_POINT ( 'NONE',  ( 80.90000000000000568, -35.04374999877096997, -97.40192378864668399 ) ) ;
#10631 = CARTESIAN_POINT ( 'NONE',  ( 232.5999999999999375, -34.16249999999999432, 96.53589838486223584 ) ) ;
#10632 = ORIENTED_EDGE ( 'NONE', *, *, #11295, .F. ) ;
#10633 = CARTESIAN_POINT ( 'NONE',  ( 231.2217848218749339, -33.32812499938548001, -47.61286128772501769 ) ) ;
#10634 = DIRECTION ( 'NONE',  ( 0.000000000000000000, 0.000000000000000000, 1.000000000000000000 ) ) ;
#10635 = CARTESIAN_POINT ( 'NONE',  ( 235.5999999999999943, -35.15624999877096002, 101.7320508075688537 ) ) ;
#10636 = CARTESIAN_POINT ( 'NONE',  ( 234.0999999999999375, -34.74374999877096570, -47.40192378864679768 ) ) ;
#10637 = CARTESIAN_POINT ( 'NONE',  ( -81.02178482187500208, -32.54062499938548569, 97.61286128772489690 ) ) ;
#10638 = ORIENTED_EDGE ( 'NONE', *, *, #17371, .T. ) ;
#10639 = EDGE_LOOP ( 'NONE', ( #12272, #15721, #8102, #2995 ) ) ;
#10640 = CARTESIAN_POINT ( 'NONE',  ( -4.000000000000000000, -0.8232339106130515116, -3.430630286862743183 ) ) ;
#10641 = CARTESIAN_POINT ( 'NONE',  ( -79.39999999999999147, -34.68750000000000000, 98.26794919243110371 ) ) ;
#10642 = ORIENTED_EDGE ( 'NONE', *, *, #16927, .F. ) ;
#10643 = CARTESIAN_POINT ( 'NONE',  ( -82.39999999999999147, -32.30624999877096570, 96.99999999999998579 ) ) ;
#10644 = LINE ( 'NONE', #7619, #14856 ) ;
#10645 = CARTESIAN_POINT ( 'NONE',  ( -83.77821517812500929, -34.67812499938548854, 102.3871387122750889 ) ) ;
#10646 = CARTESIAN_POINT ( 'NONE',  ( -82.39999999999999147, -33.48750000000000426, 103.4641016151377499 ) ) ;
#10647 =( BOUNDED_CURVE ( )  B_SPLINE_CURVE ( 2, ( #14542, #17203, #1079, #2249, #8220, #7037, #18964, #801, #12703 ),
 .UNSPECIFIED., .F., .F. ) 
 B_SPLINE_CURVE_WITH_KNOTS ( ( 3, 2, 2, 2, 3 ),
 ( 0.8125000000000000000, 0.8194444444444444198, 0.8333333333333333703, 0.8472222222222222099, 0.8541666666666668517 ),
 .UNSPECIFIED. ) 
 CURVE ( )  GEOMETRIC_REPRESENTATION_ITEM ( )  RATIONAL_B_SPLINE_CURVE ( ( 0.9330127018922194093, 0.9330127018922194093, 1.000000000000000000, 0.8660254037844387076, 1.000000000000000000, 0.8660254037844387076, 1.000000000000000000, 0.9330127018922177440, 0.9330127018922194093 ) ) 
 REPRESENTATION_ITEM ( '' )  );
#10648 = CARTESIAN_POINT ( 'NONE',  ( -82.39999999999999147, -31.18124999877096926, 103.4641016151377499 ) ) ;
#10649 = CARTESIAN_POINT ( 'NONE',  ( -82.39999999999999147, -32.58750000000000568, 102.9999999999999858 ) ) ;
#10650 = CARTESIAN_POINT ( 'NONE',  ( -83.77821517812500929, -35.12812499938548427, 102.3871387122750889 ) ) ;
#10651 = CARTESIAN_POINT ( 'NONE',  ( 235.5999999999999943, -33.41249999999999432, 101.7320508075688537 ) ) ;
#10652 = DIRECTION ( 'NONE',  ( 0.000000000000000000, 1.000000000000000000, 0.000000000000000000 ) ) ;
#10653 = CARTESIAN_POINT ( 'NONE',  ( -81.05805657947830412, -35.00000000000000711, -102.6149389257478362 ) ) ;
#10654 = CARTESIAN_POINT ( 'NONE',  ( 233.9782151781249411, -32.24062499938548143, 102.3871387122750889 ) ) ;
#10655 = VERTEX_POINT ( 'NONE', #1618 ) ;
#10656 = CARTESIAN_POINT ( 'NONE',  ( -85.15643035625001289, -32.39062499938548711, -99.99999999999998579 ) ) ;
#10657 = DIRECTION ( 'NONE',  ( 0.000000000000000000, 0.000000000000000000, 1.000000000000000000 ) ) ;
#10658 = DIRECTION ( 'NONE',  ( 0.000000000000000000, 0.000000000000000000, 1.000000000000000000 ) ) ;
#10659 = CARTESIAN_POINT ( 'NONE',  ( -85.39999999999999147, -34.97364041986484295, -101.0919042218176287 ) ) ;
#10660 = CARTESIAN_POINT ( 'NONE',  ( 229.8966310988219846, -35.00000000000002132, -49.00607337841733369 ) ) ;
#10661 = CARTESIAN_POINT ( 'NONE',  ( 233.9782151781249411, -34.94062499938547717, -47.61286128772501769 ) ) ;
#10662 = VERTEX_POINT ( 'NONE', #4544 ) ;
#10663 = VERTEX_POINT ( 'NONE', #13615 ) ;
#10664 = DIRECTION ( 'NONE',  ( 0.000000000000000000, 0.000000000000000000, 1.000000000000000000 ) ) ;
#10665 = CARTESIAN_POINT ( 'NONE',  ( -85.40000000000000568, -31.76249999999999929, 101.7320508075688679 ) ) ;
#10666 = EDGE_CURVE ( 'NONE', #14591, #4985, #1737, .T. ) ;
#10667 = CARTESIAN_POINT ( 'NONE',  ( -83.90000000000000568, -31.81874999877096855, 97.40192378864668399 ) ) ;
#10668 = CARTESIAN_POINT ( 'NONE',  ( 85.40000000000000568, -32.66250000000000142, 98.26794919243111792 ) ) ;
#10669 = CARTESIAN_POINT ( 'NONE',  ( 83.90000000000000568, -33.61874999877097281, 102.5980762113533018 ) ) ;
#10670 = CARTESIAN_POINT ( 'NONE',  ( 233.9782151781249411, -33.44062499938547717, 97.61286128772489690 ) ) ;
#10671 = CARTESIAN_POINT ( 'NONE',  ( 81.02178482187500208, -32.80312499938548854, -102.3871387122750889 ) ) ;
#10672 = CARTESIAN_POINT ( 'NONE',  ( 81.59615242270665192, -33.28259618943233278, -97.00000000000000000 ) ) ;
#10673 = CIRCLE ( 'NONE', #9111, 2.499999999999999556 ) ;
#10674 =( BOUNDED_CURVE ( )  B_SPLINE_CURVE ( 2, ( #6189, #18295, #3534, #337, #3627, #15159, #1972, #7738, #4720 ),
 .UNSPECIFIED., .F., .F. ) 
 B_SPLINE_CURVE_WITH_KNOTS ( ( 3, 2, 2, 2, 3 ),
 ( 0.7708333333333331483, 0.7777777777777777901, 0.7916666666666666297, 0.8055555555555555802, 0.8125000000000001110 ),
 .UNSPECIFIED. ) 
 CURVE ( )  GEOMETRIC_REPRESENTATION_ITEM ( )  RATIONAL_B_SPLINE_CURVE ( ( 0.9330127018922194093, 0.9330127018922177440, 1.000000000000000000, 0.8660254037844387076, 1.000000000000000000, 0.8660254037844387076, 1.000000000000000000, 0.9330127018922182991, 0.9330127018922194093 ) ) 
 REPRESENTATION_ITEM ( '' )  );
#10675 = CARTESIAN_POINT ( 'NONE',  ( 85.15643035625001289, -34.19062499938548427, -99.99999999999998579 ) ) ;
#10676 = ORIENTED_EDGE ( 'NONE', *, *, #19299, .F. ) ;
#10678 = EDGE_CURVE ( 'NONE', #6974, #7760, #17931, .T. ) ;
#10677 = CARTESIAN_POINT ( 'NONE',  ( 234.0999999999999375, -33.44999999999999574, -47.40192378864679768 ) ) ;
#10679 = CARTESIAN_POINT ( 'NONE',  ( -83.90000000000000568, -33.97500000000000853, 102.5980762113533018 ) ) ;
#10680 = CARTESIAN_POINT ( 'NONE',  ( 85.15643035624999868, -32.42812499938548854, -98.40857419181659793 ) ) ;
#10681 = ADVANCED_FACE ( 'NONE', ( #4938 ), #8683, .F. ) ;
#10682 = DIRECTION ( 'NONE',  ( 0.000000000000000000, 0.000000000000000000, 1.000000000000000000 ) ) ;
#10683 = CARTESIAN_POINT ( 'NONE',  ( -79.64356964374999848, -31.82812499938548356, 99.99999999999998579 ) ) ;
#10684 = CARTESIAN_POINT ( 'NONE',  ( 231.2217848218749339, -33.32812499938548001, -47.61286128772501769 ) ) ;
#10685 = ADVANCED_FACE ( 'NONE', ( #5176 ), #8575, .F. ) ;
#10686 = CARTESIAN_POINT ( 'NONE',  ( -84.51155491706698797, -35.14114833091483803, 98.22820877610629964 ) ) ;
#10687 = VERTEX_POINT ( 'NONE', #2235 ) ;
#10688 = CARTESIAN_POINT ( 'NONE',  ( -79.42451116572152614, -34.99876810435319641, 100.5066497421356786 ) ) ;
#10689 = CIRCLE ( 'NONE', #7262, 2.649999999999980371 ) ;
#10690 = CARTESIAN_POINT ( 'NONE',  ( 229.8435696437499587, -33.70312499938548001, 101.5914258081833879 ) ) ;
#10691 = CARTESIAN_POINT ( 'NONE',  ( -82.39999999999999147, -32.36250000000000426, 96.99999999999997158 ) ) ;
#10692 = CARTESIAN_POINT ( 'NONE',  ( -80.90000000000000568, -34.19606250001229597, 97.40192378864668399 ) ) ;
#10693 = CARTESIAN_POINT ( 'NONE',  ( -83.20384757729335945, -33.05759618943233136, -96.99999999999998579 ) ) ;
#10694 = ADVANCED_FACE ( 'NONE', ( #12688 ), #603, .F. ) ;
#10695 = CARTESIAN_POINT ( 'NONE',  ( -81.02178482187500208, -32.35312499938548569, 102.3871387122750889 ) ) ;
#10696 = CARTESIAN_POINT ( 'NONE',  ( -80.90000000000000568, -32.55000000000000426, 102.5980762113533018 ) ) ;
#10697 = CARTESIAN_POINT ( 'NONE',  ( 79.64356964375001269, -34.56562499938549138, 98.40857419181659793 ) ) ;
#10698 = CARTESIAN_POINT ( 'NONE',  ( 83.77821517812500929, -32.87812499938548427, -102.3871387122750889 ) ) ;
#10699 = CARTESIAN_POINT ( 'NONE',  ( 233.9782151781249411, -31.79062499938548214, -47.61286128772501769 ) ) ;
#10700 = CARTESIAN_POINT ( 'NONE',  ( -82.39999999999999147, -32.61562499938548854, 96.81714838363319586 ) ) ;
#10701 = CARTESIAN_POINT ( 'NONE',  ( -82.39999999999999147, -32.61562499938548854, -103.1828516163667899 ) ) ;
#10702 = AXIS2_PLACEMENT_3D ( 'NONE', #2061, #9193, #13786 ) ;
#10703 = EDGE_LOOP ( 'NONE', ( #7373, #3911 ) ) ;
#10704 = CARTESIAN_POINT ( 'NONE',  ( 82.39999999999999147, -34.55624999877096570, 103.4641016151377499 ) ) ;
#10705 = CARTESIAN_POINT ( 'NONE',  ( 4.630153689607048761, 6.577590292450083844E-16, 5.371010071662833063 ) ) ;
#10706 = CARTESIAN_POINT ( 'NONE',  ( -82.40000000000000568, -30.00000000000000355, 99.99999999999998579 ) ) ;
#10707 = CARTESIAN_POINT ( 'NONE',  ( -79.64356964375001269, -31.79062499938548569, 98.40857419181659793 ) ) ;
#10708 = CARTESIAN_POINT ( 'NONE',  ( 82.40000000000001990, -34.61250000000001137, -97.00000000000000000 ) ) ;
#10709 = EDGE_LOOP ( 'NONE', ( #15102, #6629, #3235, #10392, #3311, #10760, #19268, #18007, #18117, #9709, #4269, #13420, #7514, #10733, #10229, #4180, #6054 ) ) ;
#10710 = ADVANCED_FACE ( 'NONE', ( #13830 ), #4864, .F. ) ;
#10711 = CARTESIAN_POINT ( 'NONE',  ( -83.90000000000000568, -30.97500000000000142, -102.5980762113533018 ) ) ;
#10712 =( BOUNDED_CURVE ( )  B_SPLINE_CURVE ( 2, ( #13596, #14874, #12143, #18112, #8913, #4726, #10669, #6289, #16638 ),
 .UNSPECIFIED., .F., .F. ) 
 B_SPLINE_CURVE_WITH_KNOTS ( ( 3, 2, 2, 2, 3 ),
 ( 0.5625000000000000000, 0.5694444444444444198, 0.5833333333333333703, 0.5972222222222222099, 0.6041666666666666297 ),
 .UNSPECIFIED. ) 
 CURVE ( )  GEOMETRIC_REPRESENTATION_ITEM ( )  RATIONAL_B_SPLINE_CURVE ( ( 0.9330127018922194093, 0.9330127018922194093, 1.000000000000000000, 0.8660254037844387076, 1.000000000000000000, 0.8660254037844387076, 1.000000000000000000, 0.9330127018922198534, 0.9330127018922192983 ) ) 
 REPRESENTATION_ITEM ( '' )  );
#10713 = CARTESIAN_POINT ( 'NONE',  ( 83.95700771753406855, -35.00000000000000000, 102.5724980549417324 ) ) ;
#10714 = PLANE ( 'NONE',  #3276 ) ;
#10715 = CARTESIAN_POINT ( 'NONE',  ( 82.40000000000001990, -34.16250000000000853, 103.0000000000000000 ) ) ;
#10716 = DIRECTION ( 'NONE',  ( -1.000000000000000000, -0.000000000000000000, -0.000000000000000000 ) ) ;
#10717 = CARTESIAN_POINT ( 'NONE',  ( 229.8435696437499871, -34.34062499938547575, 98.40857419181659793 ) ) ;
#10718 = CARTESIAN_POINT ( 'NONE',  ( -79.39999999999999147, -31.93518749875867968, 98.26794919243110371 ) ) ;
#10719 = EDGE_LOOP ( 'NONE', ( #17002, #1568, #7487, #16829 ) ) ;
#10720 = DIRECTION ( 'NONE',  ( 1.387778780781445873E-15, 1.000000000000000000, 0.000000000000000000 ) ) ;
#10721 = CARTESIAN_POINT ( 'NONE',  ( 81.59615242270665192, -32.77634618820330559, -97.00000000000000000 ) ) ;
#10722 = CARTESIAN_POINT ( 'NONE',  ( 79.64356964374999848, -34.41562499938548569, 99.99999999999998579 ) ) ;
#10723 = CARTESIAN_POINT ( 'NONE',  ( 105.1999999999999744, -4.999999999999976907, 153.0000000000000000 ) ) ;
#10724 = DIRECTION ( 'NONE',  ( -0.000000000000000000, 0.000000000000000000, -1.000000000000000000 ) ) ;
#10725 = CARTESIAN_POINT ( 'NONE',  ( 85.40000000000000568, -33.95624999877097139, -101.7320508075688679 ) ) ;
#10726 = CARTESIAN_POINT ( 'NONE',  ( 82.39999999999999147, -34.83749999999999858, 97.00000000000000000 ) ) ;
#10727 = ORIENTED_EDGE ( 'NONE', *, *, #16035, .F. ) ;
#10728 = CARTESIAN_POINT ( 'NONE',  ( 229.8435696437499587, -34.26562499938548001, -48.40857419181671162 ) ) ;
#10729 = SHAPE_REPRESENTATION_RELATIONSHIP ( 'NONE' , 'NONE' ,  #19222, #9020 ) ;
#10730 = CARTESIAN_POINT ( 'NONE',  ( 232.5999999999999375, -35.23124999877096286, 103.4641016151377499 ) ) ;
#10731 = CARTESIAN_POINT ( 'NONE',  ( 235.3564303562499447, -30.89062499938548001, -51.59142580818350865 ) ) ;
#10732 = CARTESIAN_POINT ( 'NONE',  ( 232.5999999999999375, -34.61249999999999716, -53.00000000000011369 ) ) ;
#10733 = ORIENTED_EDGE ( 'NONE', *, *, #14769, .T. ) ;
#10734 = ORIENTED_EDGE ( 'NONE', *, *, #11528, .F. ) ;
#10735 = CARTESIAN_POINT ( 'NONE',  ( -81.44903907897365514, -32.00000000000000711, 97.25957015486996227 ) ) ;
#10736 = CARTESIAN_POINT ( 'NONE',  ( -85.40000000000000568, -30.88124999877096855, 98.26794919243111792 ) ) ;
#10737 = CARTESIAN_POINT ( 'NONE',  ( -82.39999999999999147, -34.83749999999999858, 103.0000000000000000 ) ) ;
#10738 = ORIENTED_EDGE ( 'NONE', *, *, #7559, .T. ) ;
#10739 = CARTESIAN_POINT ( 'NONE',  ( 99.99999999999997158, -5.200000000000008171, 150.0000000000000000 ) ) ;
#10740 = CARTESIAN_POINT ( 'NONE',  ( 231.7961524227065411, -34.08615380933862582, 97.00000000000000000 ) ) ;
#10741 = CARTESIAN_POINT ( 'NONE',  ( -84.51155386534844638, -35.25364837475780888, 98.22820752270799005 ) ) ;
#10742 = CARTESIAN_POINT ( 'NONE',  ( -83.90000000000000568, -30.76874999877097139, 102.5980762113533018 ) ) ;
#10743 = B_SPLINE_CURVE_WITH_KNOTS ( 'NONE', 3,
 ( #16961, #7780, #3572, #7874, #9532, #9143, #1721, #2110 ),
 .UNSPECIFIED., .F., .F.,
 ( 4, 2, 2, 4 ),
 ( 2.465131517390770070E-07, 0.001183067374689869946, 0.001774477805458935659, 0.002365888236228001588 ),
 .UNSPECIFIED. ) ;
#10744 = CARTESIAN_POINT ( 'NONE',  ( -80.90000000000000568, -32.79374999877096997, 97.40192378864668399 ) ) ;
#10745 = DIRECTION ( 'NONE',  ( 0.000000000000000000, 1.000000000000000000, 0.000000000000000000 ) ) ;
#10746 = DIRECTION ( 'NONE',  ( -0.000000000000000000, 0.000000000000000000, -1.000000000000000000 ) ) ;
#10747 = PRESENTATION_STYLE_ASSIGNMENT (( #18184 ) ) ;
#10748 = DIRECTION ( 'NONE',  ( 0.000000000000000000, 0.000000000000000000, 1.000000000000000000 ) ) ;
#10749 = DIRECTION ( 'NONE',  ( 0.000000000000000000, 0.000000000000000000, -1.000000000000000000 ) ) ;
#10750 = CARTESIAN_POINT ( 'NONE',  ( 235.3564303562499447, -32.57812499938547290, 98.40857419181659793 ) ) ;
#10751 = VERTEX_POINT ( 'NONE', #10808 ) ;
#10752 = CARTESIAN_POINT ( 'NONE',  ( -81.02178482187500208, -33.59062499938548285, -97.61286128772489690 ) ) ;
#10753 = CARTESIAN_POINT ( 'NONE',  ( 4.124214193018025831, 4.056676826581947282, -1.560956519390234888E-16 ) ) ;
#10754 = VERTEX_POINT ( 'NONE', #7974 ) ;
#10755 = DIRECTION ( 'NONE',  ( 0.000000000000000000, 0.000000000000000000, 1.000000000000000000 ) ) ;
#10756 = CARTESIAN_POINT ( 'NONE',  ( 246.9999999999999716, -5.000000000000004441, -100.0000000000000000 ) ) ;
#10757 = LINE ( 'NONE', #16436, #390 ) ;
#10758 = CARTESIAN_POINT ( 'NONE',  ( 229.8435696437499871, -34.60312499938547859, -48.40857419181671162 ) ) ;
#10759 = ORIENTED_EDGE ( 'NONE', *, *, #12466, .T. ) ;
#10760 = ORIENTED_EDGE ( 'NONE', *, *, #11869, .T. ) ;
#10761 = CARTESIAN_POINT ( 'NONE',  ( 82.40000000000000568, -33.43124999877096570, -102.9999999999999858 ) ) ;
#10762 = CARTESIAN_POINT ( 'NONE',  ( 79.39999999999999147, -31.12500000000000355, -99.99999999999998579 ) ) ;
#10763 = CARTESIAN_POINT ( 'NONE',  ( -80.90000000000000568, -34.59374999877096712, 97.40192378864668399 ) ) ;
#10764 = CARTESIAN_POINT ( 'NONE',  ( 79.39999999999999147, -32.88750000000000284, 101.7320508075688821 ) ) ;
#10765 = FACE_OUTER_BOUND ( 'NONE', #14570, .T. ) ;
#10766 = CARTESIAN_POINT ( 'NONE',  ( 229.8435696437499303, -34.19062499938547717, 99.99999999999998579 ) ) ;
#10767 =( BOUNDED_CURVE ( )  B_SPLINE_CURVE ( 2, ( #8567, #17567, #15717, #5369, #12781, #8193, #12678, #10044, #14333 ),
 .UNSPECIFIED., .F., .F. ) 
 B_SPLINE_CURVE_WITH_KNOTS ( ( 3, 2, 2, 2, 3 ),
 ( 0.4791666666666665186, 0.4861111111111111049, 0.5000000000000000000, 0.5138888888888888395, 0.5208333333333332593 ),
 .UNSPECIFIED. ) 
 CURVE ( )  GEOMETRIC_REPRESENTATION_ITEM ( )  RATIONAL_B_SPLINE_CURVE ( ( 0.9330127018922194093, 0.9330127018922180770, 1.000000000000000000, 0.8660254037844387076, 1.000000000000000000, 0.8660254037844387076, 1.000000000000000000, 0.9330127018922198534, 0.9330127018922192983 ) ) 
 REPRESENTATION_ITEM ( '' )  );
#10768 = CARTESIAN_POINT ( 'NONE',  ( 81.02178482187500208, -32.35312499938548569, -102.3871387122750889 ) ) ;
#10769 = FACE_OUTER_BOUND ( 'NONE', #12683, .T. ) ;
#10770 = ADVANCED_FACE ( 'NONE', ( #3478 ), #14031, .F. ) ;
#10771 = AXIS2_PLACEMENT_3D ( 'NONE', #16678, #3284, #9242 ) ;
#10772 = CARTESIAN_POINT ( 'NONE',  ( 81.02178482187500208, -33.89062499938548711, -97.61286128772489690 ) ) ;
#10773 = VERTEX_POINT ( 'NONE', #6421 ) ;
#10774 = CARTESIAN_POINT ( 'NONE',  ( 234.0999999999999375, -32.84999999999999432, -52.59807621135342970 ) ) ;
#10775 = CARTESIAN_POINT ( 'NONE',  ( -80.90000000000000568, -34.35000000000000853, 102.5980762113533018 ) ) ;
#10776 = ADVANCED_FACE ( 'NONE', ( #17064 ), #4964, .F. ) ;
#10777 = EDGE_CURVE ( 'NONE', #2466, #10773, #9243, .T. ) ;
#10778 = DIRECTION ( 'NONE',  ( -0.000000000000000000, -1.000000000000000000, -0.000000000000000000 ) ) ;
#10779 = CARTESIAN_POINT ( 'NONE',  ( -81.02178482187500208, -30.85312499938548569, 97.61286128772489690 ) ) ;
#10780 = CARTESIAN_POINT ( 'NONE',  ( 231.2217848218749339, -33.92812499938548143, -52.38713871227520968 ) ) ;
#10781 = CARTESIAN_POINT ( 'NONE',  ( -80.90000000000000568, -31.05000000000000071, 97.40192378864668399 ) ) ;
#10782 = VERTEX_POINT ( 'NONE', #13739 ) ;
#10783 = CARTESIAN_POINT ( 'NONE',  ( -85.29357727954830182, -34.99999999999999289, 100.3154961327914805 ) ) ;
#10784 = AXIS2_PLACEMENT_3D ( 'NONE', #2381, #2569, #11270 ) ;
#10785 = CARTESIAN_POINT ( 'NONE',  ( 229.8435696437499587, -34.67812499938547433, 98.40857419181659793 ) ) ;
#10786 = CARTESIAN_POINT ( 'NONE',  ( 82.39999999999999147, -30.47812499938548569, 96.81714838363319586 ) ) ;
#10787 = ADVANCED_FACE ( 'NONE', ( #18343 ), #14121, .F. ) ;
#10788 = EDGE_CURVE ( 'NONE', #12074, #14621, #5057, .T. ) ;
#10789 = CARTESIAN_POINT ( 'NONE',  ( -81.02178482187500208, -31.00312499938548783, 102.3871387122750889 ) ) ;
#10790 = CARTESIAN_POINT ( 'NONE',  ( -84.44763168836719558, -32.00000000000001421, -98.15470523285542015 ) ) ;
#10791 = CARTESIAN_POINT ( 'NONE',  ( 81.02178482187500208, -34.15312499938548285, 97.61286128772489690 ) ) ;
#10792 = AXIS2_PLACEMENT_3D ( 'NONE', #7414, #18960, #3301 ) ;
#10793 = CARTESIAN_POINT ( 'NONE',  ( 79.64356964374999848, -32.27812499938548996, -99.99999999999998579 ) ) ;
#10794 = CARTESIAN_POINT ( 'NONE',  ( 244.7999999999999545, -35.00000000000000000, 150.0000000000000000 ) ) ;
#10795 = CARTESIAN_POINT ( 'NONE',  ( -83.77821517812500929, -32.01562499938548001, 97.61286128772489690 ) ) ;
#10796 = CARTESIAN_POINT ( 'NONE',  ( -82.39999999999999147, -32.84062499938548996, -96.81714838363319586 ) ) ;
#10797 = ORIENTED_EDGE ( 'NONE', *, *, #1001, .F. ) ;
#10798 = CARTESIAN_POINT ( 'NONE',  ( 82.39999999999999147, -30.36562499938549209, 103.1828516163667899 ) ) ;
#10799 = CARTESIAN_POINT ( 'NONE',  ( 3.972066048304760955, -3.435565134476476601, -1.180968096049750393 ) ) ;
#10800 = PRESENTATION_STYLE_ASSIGNMENT (( #12077 ) ) ;
#10801 = CARTESIAN_POINT ( 'NONE',  ( -81.02178482187500208, -33.70312499938548711, 102.3871387122750889 ) ) ;
#10802 = FACE_OUTER_BOUND ( 'NONE', #6946, .T. ) ;
#10803 = ORIENTED_EDGE ( 'NONE', *, *, #6180, .F. ) ;
#10804 = CARTESIAN_POINT ( 'NONE',  ( -85.40000000000000568, -30.93750000000000355, -101.7320508075688679 ) ) ;
#10805 = PRODUCT_DEFINITION_FORMATION_WITH_SPECIFIED_SOURCE ( 'ANY', '', #10904, .NOT_KNOWN. ) ;
#10806 = CARTESIAN_POINT ( 'NONE',  ( 79.39999999999999147, -34.27499999999999858, -99.99999999999998579 ) ) ;
#10807 = CARTESIAN_POINT ( 'NONE',  ( -96.99999999999998579, -5.200000000000000178, 150.0000000000000000 ) ) ;
#10808 = CARTESIAN_POINT ( 'NONE',  ( 0.3126073911695752550, -2.020725942163798194, -3.500000000000000000 ) ) ;
#10809 = CARTESIAN_POINT ( 'NONE',  ( -1.390230914382372118, -4.043987460488664532, -3.502507215260523665 ) ) ;
#10810 = CARTESIAN_POINT ( 'NONE',  ( 231.2217848218749339, -35.12812499938548427, 102.3871387122750889 ) ) ;
#10811 = CARTESIAN_POINT ( 'NONE',  ( -84.69814161231455785, -35.39821079482706523, 98.07164704222793716 ) ) ;
#10812 = VERTEX_POINT ( 'NONE', #16773 ) ;
#10813 = LINE ( 'NONE', #1921, #12733 ) ;
#10814 = DIRECTION ( 'NONE',  ( -1.000000000000000000, 0.000000000000000000, 0.000000000000000000 ) ) ;
#10815 = CARTESIAN_POINT ( 'NONE',  ( 79.64356964374998427, -32.65312499938548285, 98.40857419181659793 ) ) ;
#10816 = CARTESIAN_POINT ( 'NONE',  ( 111.0000000000000142, 15.19999999999997797, -143.3166247903554336 ) ) ;
#10817 = CARTESIAN_POINT ( 'NONE',  ( 4.630153689607048761, 0.000000000000000000, 0.000000000000000000 ) ) ;
#10818 = CARTESIAN_POINT ( 'NONE',  ( 85.40000000000000568, -34.89374999877097139, -99.99999999999998579 ) ) ;
#10819 = EDGE_LOOP ( 'NONE', ( #2858, #15009, #7009, #951 ) ) ;
#10820 = CARTESIAN_POINT ( 'NONE',  ( 235.3564303562499447, -33.66562499938548569, -48.40857419181671162 ) ) ;
#10821 = DIRECTION ( 'NONE',  ( 1.000000000000000000, 0.000000000000000000, 0.000000000000000000 ) ) ;
#10822 = CARTESIAN_POINT ( 'NONE',  ( 233.9782151781249411, -31.90312499938548285, 102.3871387122750889 ) ) ;
#10823 = CARTESIAN_POINT ( 'NONE',  ( 231.2217848218749339, -31.52812499938548285, -47.61286128772501769 ) ) ;
#10824 = VECTOR ( 'NONE', #11709, 1000.000000000000000 ) ;
#10825 =( BOUNDED_CURVE ( )  B_SPLINE_CURVE ( 2, ( #1917, #473, #6797, #6422, #12743, #18711, #13027, #17334, #4335 ),
 .UNSPECIFIED., .F., .F. ) 
 B_SPLINE_CURVE_WITH_KNOTS ( ( 3, 2, 2, 2, 3 ),
 ( 0.4791666666666666852, 0.4861111111111111049, 0.5000000000000000000, 0.5138888888888888395, 0.5208333333333331483 ),
 .UNSPECIFIED. ) 
 CURVE ( )  GEOMETRIC_REPRESENTATION_ITEM ( )  RATIONAL_B_SPLINE_CURVE ( ( 0.9330127018922194093, 0.9330127018922196314, 1.000000000000000000, 0.8660254037844387076, 1.000000000000000000, 0.8660254037844387076, 1.000000000000000000, 0.9330127018922209636, 0.9330127018922194093 ) ) 
 REPRESENTATION_ITEM ( '' )  );
#10826 = CARTESIAN_POINT ( 'NONE',  ( -83.20384757729335945, -34.85759618943233562, 102.9999999999999716 ) ) ;
#10827 = ORIENTED_EDGE ( 'NONE', *, *, #9949, .F. ) ;
#10829 = ORIENTED_EDGE ( 'NONE', *, *, #9337, .F. ) ;
#10828 = EDGE_CURVE ( 'NONE', #6176, #2034, #12670, .T. ) ;
#10830 = CARTESIAN_POINT ( 'NONE',  ( -80.07765479365644978, -32.00000000000000000, 98.15128725331825876 ) ) ;
#10831 = CARTESIAN_POINT ( 'NONE',  ( -99.99999999999998579, 0.000000000000000000, 150.0000000000000000 ) ) ;
#10832 = CARTESIAN_POINT ( 'NONE',  ( -85.40000000000000568, -34.08749999999999858, -101.7320508075688821 ) ) ;
#10833 = VERTEX_POINT ( 'NONE', #10715 ) ;
#10834 = CARTESIAN_POINT ( 'NONE',  ( -4.000000000000000000, 0.3987449864459974846, -0.01220643443059782861 ) ) ;
#10835 = AXIS2_PLACEMENT_3D ( 'NONE', #12344, #12531, #7943 ) ;
#10836 = CARTESIAN_POINT ( 'NONE',  ( -80.90000000000000568, -33.39374999877097139, -97.40192378864668399 ) ) ;
#10837 = CARTESIAN_POINT ( 'NONE',  ( -82.39999999999999147, -34.83749999999999858, 103.4641016151377499 ) ) ;
#10838 = CARTESIAN_POINT ( 'NONE',  ( -85.40000000000000568, -34.93124999877096570, 98.26794919243111792 ) ) ;
#10839 = CARTESIAN_POINT ( 'NONE',  ( -5.384454397937118664, 6.594054843588581554E-16, -4.484454397937119197 ) ) ;
#10840 = PRESENTATION_LAYER_ASSIGNMENT (  '', '', ( #248 ) ) ;
#10841 = CARTESIAN_POINT ( 'NONE',  ( 244.7999999999999545, -35.00000000000000000, 150.0000000000000000 ) ) ;
#10842 = CARTESIAN_POINT ( 'NONE',  ( 3.958484000407190617, 3.734437307742054735, 0.5317648453100325412 ) ) ;
#10843 = CARTESIAN_POINT ( 'NONE',  ( 231.2217848218749339, -33.36562499938548143, 97.61286128772489690 ) ) ;
#10844 = CARTESIAN_POINT ( 'NONE',  ( 231.2217848218749339, -32.76562499938548001, 102.3871387122750889 ) ) ;
#10845 = ORIENTED_EDGE ( 'NONE', *, *, #19313, .F. ) ;
#10846 = EDGE_CURVE ( 'NONE', #2207, #17768, #9417, .T. ) ;
#10847 = CIRCLE ( 'NONE', #12090, 2.199999999999993516 ) ;
#10848 = CARTESIAN_POINT ( 'NONE',  ( 229.5999999999999375, -31.29374999877096286, 99.99999999999998579 ) ) ;
#10849 = FACE_BOUND ( 'NONE', #5918, .T. ) ;
#10850 = VERTEX_POINT ( 'NONE', #1134 ) ;
#10851 = CARTESIAN_POINT ( 'NONE',  ( -81.59615242270662350, -33.46740381056766722, -96.99999999999998579 ) ) ;
#10852 = CARTESIAN_POINT ( 'NONE',  ( -82.39999999999999147, -31.91249999999999787, 96.99999999999998579 ) ) ;
#10853 = CARTESIAN_POINT ( 'NONE',  ( 82.40000000000000568, -30.00000000000000355, 99.99999999999998579 ) ) ;
#10854 = ORIENTED_EDGE ( 'NONE', *, *, #5113, .T. ) ;
#10855 = CARTESIAN_POINT ( 'NONE',  ( 82.40000000000001990, -33.26250000000000284, 103.0000000000000000 ) ) ;
#10856 = VECTOR ( 'NONE', #2581, 1000.000000000000000 ) ;
#10857 = VECTOR ( 'NONE', #1781, 1000.000000000000000 ) ;
#10858 = ORIENTED_EDGE ( 'NONE', *, *, #11127, .F. ) ;
#10859 = EDGE_LOOP ( 'NONE', ( #16913, #8670, #17405, #2232 ) ) ;
#10860 = CARTESIAN_POINT ( 'NONE',  ( 111.5000000000000142, 12.69999999999998508, 110.0000000000000142 ) ) ;
#10861 = CARTESIAN_POINT ( 'NONE',  ( 83.90000000000000568, -30.07499999999999929, -97.40192378864668399 ) ) ;
#10862 = DIRECTION ( 'NONE',  ( 1.000000000000000000, -4.625929269271214620E-17, 4.415659757031858318E-14 ) ) ;
#10863 = CARTESIAN_POINT ( 'NONE',  ( -79.39999999999999147, -35.15624999877096712, 101.7320508075688537 ) ) ;
#10864 = LINE ( 'NONE', #18591, #3689 ) ;
#10865 = CARTESIAN_POINT ( 'NONE',  ( -2.855764796983342624, 2.970025579236414082, -0.09382832055445475272 ) ) ;
#10866 = CARTESIAN_POINT ( 'NONE',  ( 85.15643035625001289, -33.36562499938548854, -101.5914258081833879 ) ) ;
#10867 = AXIS2_PLACEMENT_3D ( 'NONE', #6481, #7644, #9399 ) ;
#10868 = CARTESIAN_POINT ( 'NONE',  ( 84.28136653320187577, -32.00000000000000000, -97.98546077809228905 ) ) ;
#10869 = CARTESIAN_POINT ( 'NONE',  ( -83.77821517812500929, -33.36562499938548854, 97.61286128772489690 ) ) ;
#10870 = CARTESIAN_POINT ( 'NONE',  ( 79.64356964375001269, -33.10312499938549280, -101.5914258081833879 ) ) ;
#10871 = ORIENTED_EDGE ( 'NONE', *, *, #17157, .T. ) ;
#10872 = CARTESIAN_POINT ( 'NONE',  ( 232.5999999999999375, -32.81249999999999289, -53.46410161513786363 ) ) ;
#10873 = FACE_OUTER_BOUND ( 'NONE', #4434, .T. ) ;
#10874 = CARTESIAN_POINT ( 'NONE',  ( -82.39999999999999147, -31.01249999999999929, 96.99999999999998579 ) ) ;
#10875 = CARTESIAN_POINT ( 'NONE',  ( 232.5999999999999375, -29.99999999999999645, -50.00000000000011369 ) ) ;
#10876 = CARTESIAN_POINT ( 'NONE',  ( -85.15643035625001289, -32.50312499938548427, 99.99999999999998579 ) ) ;
#10877 = CARTESIAN_POINT ( 'NONE',  ( 233.9782151781249411, -32.20312499938548001, -52.38713871227520968 ) ) ;
#10878 = CARTESIAN_POINT ( 'NONE',  ( -83.90000000000000568, -33.07500000000000284, 102.5980762113533018 ) ) ;
#10879 = ORIENTED_EDGE ( 'NONE', *, *, #13997, .T. ) ;
#10880 = CARTESIAN_POINT ( 'NONE',  ( -85.24876232368484352, -35.00000000000000000, 100.5466586069497623 ) ) ;
#10881 =( BOUNDED_CURVE ( )  B_SPLINE_CURVE ( 2, ( #11100, #10721, #12288, #14126, #16685, #7791, #17068, #4870, #15409 ),
 .UNSPECIFIED., .F., .F. ) 
 B_SPLINE_CURVE_WITH_KNOTS ( ( 3, 2, 2, 2, 3 ),
 ( 0.4374999999999999445, 0.4444444444444444198, 0.4583333333333333148, 0.4722222222222222099, 0.4791666666666666297 ),
 .UNSPECIFIED. ) 
 CURVE ( )  GEOMETRIC_REPRESENTATION_ITEM ( )  RATIONAL_B_SPLINE_CURVE ( ( 0.9330127018922192983, 0.9330127018922187432, 1.000000000000000000, 0.8660254037844387076, 1.000000000000000000, 0.8660254037844387076, 1.000000000000000000, 0.9330127018922196314, 0.9330127018922194093 ) ) 
 REPRESENTATION_ITEM ( '' )  );
#10882 = ADVANCED_BREP_SHAPE_REPRESENTATION ( '', ( #1125, #10540 ), #19229 ) ;
#10883 = CARTESIAN_POINT ( 'NONE',  ( 79.90595866893272614, -34.99999999999998579, 98.81289630734771379 ) ) ;
#10884 = CARTESIAN_POINT ( 'NONE',  ( 85.15643035624999868, -30.17812499938548498, 101.5914258081833879 ) ) ;
#10885 = ADVANCED_FACE ( 'NONE', ( #1233 ), #15986, .F. ) ;
#10886 = FACE_OUTER_BOUND ( 'NONE', #4926, .T. ) ;
#10887 = CARTESIAN_POINT ( 'NONE',  ( -83.77821517812500929, -30.32812499938548711, 97.61286128772489690 ) ) ;
#10888 = CARTESIAN_POINT ( 'NONE',  ( 117.5000000000000142, 12.69999999999998508, 50.00000000000001421 ) ) ;
#10889 = CARTESIAN_POINT ( 'NONE',  ( 79.64356964375001269, -30.40312499938548285, 98.40857419181659793 ) ) ;
#10890 = CARTESIAN_POINT ( 'NONE',  ( 85.15643035624999868, -32.46562499938548996, -101.5914258081833879 ) ) ;
#10891 = CARTESIAN_POINT ( 'NONE',  ( 229.8435696437499871, -30.62812499938547717, -51.59142580818350865 ) ) ;
#10892 = CARTESIAN_POINT ( 'NONE',  ( -83.77821517812500929, -33.92812499938548854, 97.61286128772489690 ) ) ;
#10893 = CARTESIAN_POINT ( 'NONE',  ( -79.64356964375001269, -33.21562499938548996, -98.40857419181659793 ) ) ;
#10894 = EDGE_LOOP ( 'NONE', ( #4741, #7138, #12325, #117 ) ) ;
#10895 = CARTESIAN_POINT ( 'NONE',  ( 85.15643035624999868, -33.36562499938548854, 98.40857419181659793 ) ) ;
#10896 = CARTESIAN_POINT ( 'NONE',  ( 231.0999999999999375, -32.17499999999999716, 102.5980762113533018 ) ) ;
#10897 = CARTESIAN_POINT ( 'NONE',  ( -83.77821517812500929, -30.96562499938548640, 102.3871387122750889 ) ) ;
#10898 = EDGE_CURVE ( 'NONE', #2034, #14891, #14407, .T. ) ;
#10899 = CARTESIAN_POINT ( 'NONE',  ( -85.15643035625001289, -32.95312499938548711, 99.99999999999998579 ) ) ;
#10900 = EDGE_CURVE ( 'NONE', #7039, #3084, #18287, .T. ) ;
#10901 = DIRECTION ( 'NONE',  ( 0.000000000000000000, 0.000000000000000000, -1.000000000000000000 ) ) ;
#10902 = ORIENTED_EDGE ( 'NONE', *, *, #1230, .F. ) ;
#10903 = CARTESIAN_POINT ( 'NONE',  ( -82.39999999999999147, -33.71249999999999858, -103.4641016151377499 ) ) ;
#10904 = PRODUCT ( 'workbench', 'workbench', '', ( #9657 ) ) ;
#10905 = CARTESIAN_POINT ( 'NONE',  ( -79.39999999999999147, -32.45624999877097139, 101.7320508075688537 ) ) ;
#10906 = CARTESIAN_POINT ( 'NONE',  ( -3.510273485745307287, -2.827716139362669967, -3.610536846335890004 ) ) ;
#10907 = DIRECTION ( 'NONE',  ( -0.000000000000000000, 0.000000000000000000, 1.000000000000000000 ) ) ;
#10908 = EDGE_CURVE ( 'NONE', #2292, #7532, #10058, .T. ) ;
#10909 = CARTESIAN_POINT ( 'NONE',  ( 233.9782151781249411, -33.70312499938548001, 102.3871387122750889 ) ) ;
#10910 = CARTESIAN_POINT ( 'NONE',  ( -83.90000000000000568, -33.47268749875867400, 102.5980762113533018 ) ) ;
#10911 = ORIENTED_EDGE ( 'NONE', *, *, #8740, .F. ) ;
#10912 = DIRECTION ( 'NONE',  ( 1.000000000000000000, 0.000000000000000000, 0.000000000000000000 ) ) ;
#10913 = CARTESIAN_POINT ( 'NONE',  ( -83.20384757729337366, -34.35134618820330843, 103.0000000000000000 ) ) ;
#10914 = FACE_OUTER_BOUND ( 'NONE', #3408, .T. ) ;
#10915 = CARTESIAN_POINT ( 'NONE',  ( 81.59615242270665192, -34.18259618943233136, 103.0000000000000000 ) ) ;
#10916 = CARTESIAN_POINT ( 'NONE',  ( -83.90000000000000568, -34.36874999877097281, 102.5980762113533018 ) ) ;
#10917 = CARTESIAN_POINT ( 'NONE',  ( 85.15643035624999868, -32.46562499938548996, -101.5914258081833879 ) ) ;
#10918 = DIRECTION ( 'NONE',  ( -0.000000000000000000, 0.000000000000000000, 1.000000000000000000 ) ) ;
#10919 = VERTEX_POINT ( 'NONE', #8644 ) ;
#10920 = CARTESIAN_POINT ( 'NONE',  ( 85.40000000000000568, -30.43124999877096926, 101.7320508075688679 ) ) ;
#10921 =( NAMED_UNIT ( * ) PLANE_ANGLE_UNIT ( ) SI_UNIT ( $, .RADIAN. ) );
#10922 = CARTESIAN_POINT ( 'NONE',  ( 229.8435696437499871, -32.99062499938548143, 98.40857419181659793 ) ) ;
#10923 = CARTESIAN_POINT ( 'NONE',  ( 232.5999999999999375, -31.26562499938548356, -53.18285161636690361 ) ) ;
#10924 = ADVANCED_FACE ( 'NONE', ( #7093 ), #12046, .T. ) ;
#10925 = CARTESIAN_POINT ( 'NONE',  ( -82.39999999999999147, -34.30312499938548143, 96.81714838363319586 ) ) ;
#10926 = CARTESIAN_POINT ( 'NONE',  ( -82.39999999999999147, -32.81250000000000000, -103.0000000000000000 ) ) ;
#10927 = ORIENTED_EDGE ( 'NONE', *, *, #13066, .F. ) ;
#10928 = VERTEX_POINT ( 'NONE', #14219 ) ;
#10929 = CARTESIAN_POINT ( 'NONE',  ( -80.80006050682004570, -32.00000000000000711, 97.54622936382074272 ) ) ;
#10930 = EDGE_CURVE ( 'NONE', #9169, #12702, #8293, .T. ) ;
#10931 = CARTESIAN_POINT ( 'NONE',  ( 232.5999999999999375, -29.99999999999999645, -53.00000000000012079 ) ) ;
#10932 = CARTESIAN_POINT ( 'NONE',  ( -83.90000000000000568, -33.67500000000000426, -102.5980762113533018 ) ) ;
#10933 = ORIENTED_EDGE ( 'NONE', *, *, #2648, .T. ) ;
#10934 = CARTESIAN_POINT ( 'NONE',  ( -83.90000000000000568, -31.21874999877097068, 102.5980762113533018 ) ) ;
#10935 = CARTESIAN_POINT ( 'NONE',  ( -79.39999999999999147, -33.31874999877096855, -99.99999999999998579 ) ) ;
#10936 = DIRECTION ( 'NONE',  ( 1.000000000000000000, -1.387778780781445676E-15, -2.407412430484046130E-31 ) ) ;
#10937 = CARTESIAN_POINT ( 'NONE',  ( -79.39999999999999147, -31.51874999877096784, 99.99999999999998579 ) ) ;
#10938 = CARTESIAN_POINT ( 'NONE',  ( -83.90000000000000568, -34.51874999877097139, 97.40192378864668399 ) ) ;
#10939 = CARTESIAN_POINT ( 'NONE',  ( 244.7999999999999545, -29.80000000000002203, 147.7999999999999829 ) ) ;
#10940 = ADVANCED_FACE ( 'NONE', ( #2403 ), #957, .T. ) ;
#10941 = CARTESIAN_POINT ( 'NONE',  ( 235.3564303562499447, -33.51562499938548001, 99.99999999999998579 ) ) ;
#10942 = ORIENTED_EDGE ( 'NONE', *, *, #10956, .F. ) ;
#10943 = CARTESIAN_POINT ( 'NONE',  ( 231.0999999999999375, -31.21874999877096357, 102.5980762113533018 ) ) ;
#10944 = DIRECTION ( 'NONE',  ( 1.000000000000000000, -4.625929269271485174E-17, 0.000000000000000000 ) ) ;
#10945 = ORIENTED_EDGE ( 'NONE', *, *, #4451, .F. ) ;
#10946 = FACE_OUTER_BOUND ( 'NONE', #19085, .T. ) ;
#10947 = CARTESIAN_POINT ( 'NONE',  ( 0.000000000000000000, -3.031088913245533867, -1.750000000000002220 ) ) ;
#10948 = PRODUCT_DEFINITION_CONTEXT ( 'detailed design', #1844, 'design' ) ;
#10949 = CARTESIAN_POINT ( 'NONE',  ( -1.393927851585477606, 4.043713361053528743, -3.526374918436835149 ) ) ;
#10950 = ORIENTED_EDGE ( 'NONE', *, *, #101, .T. ) ;
#10951 = CYLINDRICAL_SURFACE ( 'NONE', #11946, 3.000000000000002665 ) ;
#10952 = ORIENTED_EDGE ( 'NONE', *, *, #7977, .F. ) ;
#10953 = ORIENTED_EDGE ( 'NONE', *, *, #11156, .F. ) ;
#10954 = CARTESIAN_POINT ( 'NONE',  ( -80.80636817121812498, -31.99999999999999289, 102.4696265554868688 ) ) ;
#10955 = CARTESIAN_POINT ( 'NONE',  ( 85.15643035624999868, -34.60312499938548569, -101.5914258081833879 ) ) ;
#10956 = EDGE_CURVE ( 'NONE', #16985, #8815, #9943, .T. ) ;
#10957 = CARTESIAN_POINT ( 'NONE',  ( -4.000000000000000000, 0.000000000000000000, 0.000000000000000000 ) ) ;
#10958 = CARTESIAN_POINT ( 'NONE',  ( -85.40000000000000568, -34.44374999877096855, 99.99999999999998579 ) ) ;
#10959 = DIRECTION ( 'NONE',  ( -0.9396926207859138680, 0.000000000000000000, -0.3420201433256536139 ) ) ;
#10960 = CARTESIAN_POINT ( 'NONE',  ( 80.90000000000000568, -33.39374999877097139, 97.40192378864668399 ) ) ;
#10961 = CARTESIAN_POINT ( 'NONE',  ( 82.39999999999999147, -32.39062499938548711, -103.1828516163667899 ) ) ;
#10962 = CARTESIAN_POINT ( 'NONE',  ( 3.806834918298644066, -4.336808689942017736E-15, -3.500000000000000000 ) ) ;
#10963 = CARTESIAN_POINT ( 'NONE',  ( -79.64356964375001269, -32.65312499938548285, 101.5914258081833879 ) ) ;
#10964 = CARTESIAN_POINT ( 'NONE',  ( 83.77821517812500929, -33.81562499938548427, -97.61286128772489690 ) ) ;
#10965 = ORIENTED_EDGE ( 'NONE', *, *, #11966, .F. ) ;
#10966 = CARTESIAN_POINT ( 'NONE',  ( 231.0999999999999375, -31.72499999999999787, -47.40192378864679768 ) ) ;
#10967 = CARTESIAN_POINT ( 'NONE',  ( -85.40000000000000568, -34.53750000000000142, 98.26794919243111792 ) ) ;
#10968 = CARTESIAN_POINT ( 'NONE',  ( -82.40000000000000568, -34.10624999877096997, 96.99999999999998579 ) ) ;
#10969 = CARTESIAN_POINT ( 'NONE',  ( -79.64356964374999848, -30.92812499938548498, 99.99999999999998579 ) ) ;
#10970 = CARTESIAN_POINT ( 'NONE',  ( 235.3564303562499447, -33.66562499938548569, -48.40857419181671162 ) ) ;
#10971 = CARTESIAN_POINT ( 'NONE',  ( -80.90000000000000568, -32.85000000000000142, 97.40192378864668399 ) ) ;
#10972 = VERTEX_POINT ( 'NONE', #10125 ) ;
#10973 = CARTESIAN_POINT ( 'NONE',  ( -81.29668248076569625, -34.99857710348262430, 102.8092562322720198 ) ) ;
#10974 = CARTESIAN_POINT ( 'NONE',  ( 3.972709601346592123, 3.429395227388311707, 1.191688283765306000 ) ) ;
#10975 = CARTESIAN_POINT ( 'NONE',  ( 79.64356964375001269, -31.75312499938548427, 98.40857419181659793 ) ) ;
#10976 = VECTOR ( 'NONE', #5171, 1000.000000000000000 ) ;
#10977 = VECTOR ( 'NONE', #309, 1000.000000000000000 ) ;
#10978 = CARTESIAN_POINT ( 'NONE',  ( 233.4038475772933339, -34.63259618943233420, 97.00000000000000000 ) ) ;
#10979 = CARTESIAN_POINT ( 'NONE',  ( -85.15643035625001289, -31.64062499938548356, 98.40857419181659793 ) ) ;
#10980 = CARTESIAN_POINT ( 'NONE',  ( -81.02178482187500208, -32.65312499938548996, -102.3871387122750889 ) ) ;
#10981 = CARTESIAN_POINT ( 'NONE',  ( 81.02178482187500208, -30.44062499938548783, 97.61286128772489690 ) ) ;
#10982 = CARTESIAN_POINT ( 'NONE',  ( 79.64356964375001269, -31.86562499938548143, -101.5914258081833879 ) ) ;
#10983 = CARTESIAN_POINT ( 'NONE',  ( 233.9782151781249411, -30.89062499938548001, -47.61286128772501769 ) ) ;
#10984 = CARTESIAN_POINT ( 'NONE',  ( -83.77821517812500929, -33.32812499938548711, 102.3871387122750889 ) ) ;
#10985 = CARTESIAN_POINT ( 'NONE',  ( -85.15643035624999868, -34.71562499938548285, -98.40857419181659793 ) ) ;
#10986 = ADVANCED_FACE ( 'NONE', ( #4259 ), #5449, .F. ) ;
#10987 = ORIENTED_EDGE ( 'NONE', *, *, #10898, .F. ) ;
#10988 = CARTESIAN_POINT ( 'NONE',  ( 85.15643035625001289, -32.50312499938548427, 99.99999999999998579 ) ) ;
#10989 = CARTESIAN_POINT ( 'NONE',  ( 3.878096787214418306, -3.381939201670154826, -1.142309474598376395 ) ) ;
#10990 =( GEOMETRIC_REPRESENTATION_CONTEXT ( 3 ) GLOBAL_UNCERTAINTY_ASSIGNED_CONTEXT ( ( #947 ) ) GLOBAL_UNIT_ASSIGNED_CONTEXT ( ( #8507, #14657, #7150 ) ) REPRESENTATION_CONTEXT ( 'NONE', 'WORKASPACE' ) );
#10991 =( BOUNDED_CURVE ( )  B_SPLINE_CURVE ( 2, ( #4657, #16192, #17844, #2984, #1242, #2800, #7194, #4363, #16282 ),
 .UNSPECIFIED., .F., .F. ) 
 B_SPLINE_CURVE_WITH_KNOTS ( ( 3, 2, 2, 2, 3 ),
 ( 0.8125000000000000000, 0.8194444444444444198, 0.8333333333333333703, 0.8472222222222222099, 0.8530683953269213582 ),
 .UNSPECIFIED. ) 
 CURVE ( )  GEOMETRIC_REPRESENTATION_ITEM ( )  RATIONAL_B_SPLINE_CURVE ( ( 0.9330127018922194093, 0.9330127018922194093, 1.000000000000000000, 0.8660254037844387076, 1.000000000000000000, 0.8660254037844387076, 1.000000000000000000, 0.9436068149601996025, 0.9346881722405915305 ) ) 
 REPRESENTATION_ITEM ( '' )  );
#10992 = CARTESIAN_POINT ( 'NONE',  ( -82.39999999999999147, -31.37812499938548427, 103.1828516163667899 ) ) ;
#10993 = VECTOR ( 'NONE', #18959, 1000.000000000000000 ) ;
#10994 = CARTESIAN_POINT ( 'NONE',  ( -79.64356964375001269, -34.49062499938548854, 98.40857419181659793 ) ) ;
#10995 = CARTESIAN_POINT ( 'NONE',  ( -82.40000000000000568, -35.00000000000000000, 99.99999999999998579 ) ) ;
#10996 = VERTEX_POINT ( 'NONE', #17647 ) ;
#10997 = CARTESIAN_POINT ( 'NONE',  ( -85.40000000000000568, -32.66250000000000142, -98.26794919243111792 ) ) ;
#10998 = DIRECTION ( 'NONE',  ( 0.000000000000000000, 0.000000000000000000, 1.000000000000000000 ) ) ;
#10999 = DIRECTION ( 'NONE',  ( 1.000000000000000000, 0.000000000000000000, -0.000000000000000000 ) ) ;
#11000 = CARTESIAN_POINT ( 'NONE',  ( 232.5999999999999375, -34.19062499938547717, 103.1828516163667899 ) ) ;
#11001 = CARTESIAN_POINT ( 'NONE',  ( -85.40000000000000568, -34.44768749875867542, 99.99999999999998579 ) ) ;
#11002 = ORIENTED_EDGE ( 'NONE', *, *, #15245, .T. ) ;
#11003 = DIRECTION ( 'NONE',  ( 0.000000000000000000, -0.000000000000000000, 1.000000000000000000 ) ) ;
#11004 = CARTESIAN_POINT ( 'NONE',  ( -85.40000000000000568, -33.50624999877096855, -98.26794919243111792 ) ) ;
#11005 = LINE ( 'NONE', #16973, #5889 ) ;
#11006 = VECTOR ( 'NONE', #2019, 1000.000000000000000 ) ;
#11007 = CARTESIAN_POINT ( 'NONE',  ( 112.8867513459481984, 10.19999999999997264, -150.0000000000000000 ) ) ;
#11008 = CARTESIAN_POINT ( 'NONE',  ( 82.39999999999999147, -31.26562499938549067, -96.81714838363319586 ) ) ;
#11009 = CARTESIAN_POINT ( 'NONE',  ( 94.79999999999995453, -32.00000000000000000, -150.0000000000000000 ) ) ;
#11010 = EDGE_CURVE ( 'NONE', #6176, #12057, #14409, .T. ) ;
#11011 = ORIENTED_EDGE ( 'NONE', *, *, #17240, .T. ) ;
#11012 = CARTESIAN_POINT ( 'NONE',  ( 235.3564303562499447, -34.56562499938547717, -48.40857419181671162 ) ) ;
#11013 = APPLICATION_PROTOCOL_DEFINITION ( 'draft international standard', 'automotive_design', 1998, #6962 ) ;
#11014 = CARTESIAN_POINT ( 'NONE',  ( 235.3564303562499447, -31.34062499938548285, 98.40857419181659793 ) ) ;
#11015 = CARTESIAN_POINT ( 'NONE',  ( 233.9782151781249411, -31.75312499938547717, -52.38713871227520968 ) ) ;
#11016 = EDGE_CURVE ( 'NONE', #6590, #2826, #6911, .T. ) ;
#11017 = CARTESIAN_POINT ( 'NONE',  ( -81.02178482187500208, -34.04062499938548569, 102.3871387122750889 ) ) ;
#11018 = CARTESIAN_POINT ( 'NONE',  ( 234.0999999999999375, -34.64999999999999147, -52.59807621135342970 ) ) ;
#11019 = ORIENTED_EDGE ( 'NONE', *, *, #9014, .F. ) ;
#11020 = VERTEX_POINT ( 'NONE', #1137 ) ;
#11021 = CARTESIAN_POINT ( 'NONE',  ( -85.15643035624999868, -30.62812499938548427, -101.5914258081833879 ) ) ;
#11022 = B_SPLINE_CURVE_WITH_KNOTS ( 'NONE', 3,
 ( #12512, #15447, #18479, #2059, #8017, #9583, #8310, #13976 ),
 .UNSPECIFIED., .F., .F.,
 ( 4, 2, 2, 4 ),
 ( 2.465131517071610173E-07, 0.001183067374689837636, 0.001774477805458902699, 0.002365888236227967761 ),
 .UNSPECIFIED. ) ;
#11023 = CARTESIAN_POINT ( 'NONE',  ( -83.90000000000000568, -30.76874999877097139, 102.5980762113533018 ) ) ;
#11024 = DIRECTION ( 'NONE',  ( -1.000000000000000000, 0.000000000000000000, -0.000000000000000000 ) ) ;
#11025 = EDGE_LOOP ( 'NONE', ( #15341, #2682, #5190, #2973, #3533 ) ) ;
#11026 = CARTESIAN_POINT ( 'NONE',  ( 85.15643035625001289, -34.30312499938548854, 99.99999999999998579 ) ) ;
#11027 = CARTESIAN_POINT ( 'NONE',  ( -79.39999999999999147, -32.83124999877097139, -101.7320508075688821 ) ) ;
#11028 = CARTESIAN_POINT ( 'NONE',  ( 113.0000000000000142, 10.19999999999995310, 50.00000000000001421 ) ) ;
#11029 = CARTESIAN_POINT ( 'NONE',  ( -85.40000000000000568, -31.74374999877096926, 99.99999999999998579 ) ) ;
#11030 = AXIS2_PLACEMENT_3D ( 'NONE', #4841, #1616, #13903 ) ;
#11031 = CARTESIAN_POINT ( 'NONE',  ( -80.90000000000000568, -35.19374999877096855, 102.5980762113533018 ) ) ;
#11032 = CARTESIAN_POINT ( 'NONE',  ( -85.40000000000000568, -32.25000000000000000, 99.99999999999998579 ) ) ;
#11033 = EDGE_CURVE ( 'NONE', #13093, #18033, #14665, .T. ) ;
#11034 = DIRECTION ( 'NONE',  ( 1.000000000000000000, -0.000000000000000000, -2.407412430484046130E-31 ) ) ;
#11035 = DIRECTION ( 'NONE',  ( -0.000000000000000000, 0.000000000000000000, -1.000000000000000000 ) ) ;
#11036 = CARTESIAN_POINT ( 'NONE',  ( 235.3564303562499447, -34.86562499938547433, 99.99999999999998579 ) ) ;
#11037 = EDGE_CURVE ( 'NONE', #3413, #4556, #16092, .T. ) ;
#11038 = VERTEX_POINT ( 'NONE', #4750 ) ;
#11039 = CARTESIAN_POINT ( 'NONE',  ( 81.02178482187500208, -32.69062499938548427, -102.3871387122750889 ) ) ;
#11040 = CARTESIAN_POINT ( 'NONE',  ( 229.5999999999999375, -30.80624999877096215, 101.7320508075688679 ) ) ;
#11041 = CARTESIAN_POINT ( 'NONE',  ( 4.142654963991903472, 4.070796997468637102, -1.539416769003468026E-16 ) ) ;
#11042 = ORIENTED_EDGE ( 'NONE', *, *, #17017, .F. ) ;
#11043 = PLANE ( 'NONE',  #19269 ) ;
#11044 = DIRECTION ( 'NONE',  ( 0.000000000000000000, 0.000000000000000000, -1.000000000000000000 ) ) ;
#11045 = DIRECTION ( 'NONE',  ( -0.000000000000000000, 0.000000000000000000, -1.000000000000000000 ) ) ;
#11046 = ORIENTED_EDGE ( 'NONE', *, *, #4026, .F. ) ;
#11047 = CARTESIAN_POINT ( 'NONE',  ( 99.99999999999997158, -5.200000000000008171, -100.0000000000000000 ) ) ;
#11048 = CARTESIAN_POINT ( 'NONE',  ( 232.5999999999999375, -33.88124999877096855, -47.00000000000011369 ) ) ;
#11049 = ORIENTED_EDGE ( 'NONE', *, *, #11373, .T. ) ;
#11050 = CARTESIAN_POINT ( 'NONE',  ( 232.5999999999999375, -33.48749999999999716, -47.00000000000011369 ) ) ;
#11051 = CARTESIAN_POINT ( 'NONE',  ( 85.40000000000000568, -31.35000000000000142, -99.99999999999998579 ) ) ;
#11052 = CARTESIAN_POINT ( 'NONE',  ( -82.39999999999999147, -34.10624999877096997, 96.53589838486223584 ) ) ;
#11053 = CARTESIAN_POINT ( 'NONE',  ( -83.90000000000000568, -34.57106250001229597, 97.40192378864668399 ) ) ;
#11054 = CARTESIAN_POINT ( 'NONE',  ( -80.90000000000000568, -33.24374999877097281, 97.40192378864668399 ) ) ;
#11055 = CARTESIAN_POINT ( 'NONE',  ( 231.0999999999999375, -33.07499999999999574, 102.5980762113533018 ) ) ;
#11056 = CARTESIAN_POINT ( 'NONE',  ( 81.02178482187500208, -32.20312499938548711, -97.61286128772489690 ) ) ;
#11057 = CARTESIAN_POINT ( 'NONE',  ( 82.40000000000000568, -30.00000000000000355, -103.0000000000000000 ) ) ;
#11058 = CARTESIAN_POINT ( 'NONE',  ( -83.77821517812500929, -32.46562499938548285, 97.61286128772489690 ) ) ;
#11059 = CARTESIAN_POINT ( 'NONE',  ( 83.77821517812500929, -33.66562499938548569, -102.3871387122750889 ) ) ;
#11060 = VERTEX_POINT ( 'NONE', #13525 ) ;
#11061 = CARTESIAN_POINT ( 'NONE',  ( 229.5999999999999375, -34.91249999999999432, -48.26794919243123161 ) ) ;
#11062 = ADVANCED_FACE ( 'NONE', ( #13338 ), #5924, .T. ) ;
#11063 = SURFACE_STYLE_FILL_AREA ( #18503 ) ;
#11064 = PRODUCT_DEFINITION_SHAPE ( 'NONE', 'NONE',  #19325 ) ;
#11065 = CARTESIAN_POINT ( 'NONE',  ( 82.40000000000000568, -33.03750000000000142, -102.9999999999999858 ) ) ;
#11066 = CARTESIAN_POINT ( 'NONE',  ( 229.8435696437499303, -32.50312499938547717, 99.99999999999998579 ) ) ;
#11067 = CARTESIAN_POINT ( 'NONE',  ( -85.15643035624999868, -31.11562499938548854, 101.5914258081833879 ) ) ;
#11068 = CARTESIAN_POINT ( 'NONE',  ( 235.3564303562499447, -32.24062499938548143, -51.59142580818350865 ) ) ;
#11069 = CARTESIAN_POINT ( 'NONE',  ( -79.39999999999999147, -32.43750000000000000, 98.26794919243110371 ) ) ;
#11070 = ORIENTED_EDGE ( 'NONE', *, *, #412, .T. ) ;
#11071 = CARTESIAN_POINT ( 'NONE',  ( -81.28560337669112812, -35.00129552118395537, 97.20965008810277652 ) ) ;
#11072 = EDGE_CURVE ( 'NONE', #9205, #11379, #18328, .T. ) ;
#11073 = CYLINDRICAL_SURFACE ( 'NONE', #18177, 7.000000000000006217 ) ;
#11074 = CARTESIAN_POINT ( 'NONE',  ( 85.15643035624999868, -31.97812499938548925, 101.5914258081833879 ) ) ;
#11075 = AXIS2_PLACEMENT_3D ( 'NONE', #18464, #4693, #15042 ) ;
#11076 = CARTESIAN_POINT ( 'NONE',  ( 81.59615242270663771, -32.11740381056766580, -103.0000000000000000 ) ) ;
#11077 = CARTESIAN_POINT ( 'NONE',  ( -79.64356964374998427, -31.79062499938548925, 98.40857419181659793 ) ) ;
#11078 = CARTESIAN_POINT ( 'NONE',  ( 3.973110223768738791, 0.6864646529411682074, 3.565797985667475967 ) ) ;
#11079 = CARTESIAN_POINT ( 'NONE',  ( 81.02178482187500208, -31.64062499938548356, 102.3871387122750889 ) ) ;
#11080 = CARTESIAN_POINT ( 'NONE',  ( 79.64356964375001269, -31.34062499938548640, -98.40857419181659793 ) ) ;
#11081 = CARTESIAN_POINT ( 'NONE',  ( 229.8435696437499871, -32.87812499938547717, -51.59142580818350865 ) ) ;
#11082 = CARTESIAN_POINT ( 'NONE',  ( -81.02178482187500208, -33.70312499938548711, 102.3871387122750889 ) ) ;
#11083 = CARTESIAN_POINT ( 'NONE',  ( -85.15643035624999868, -32.54062499938548569, -101.5914258081833879 ) ) ;
#11084 = VERTEX_POINT ( 'NONE', #7282 ) ;
#11085 = CARTESIAN_POINT ( 'NONE',  ( 83.77821517812500929, -32.12812499938548427, 102.3871387122750889 ) ) ;
#11086 = LINE ( 'NONE', #3669, #16786 ) ;
#11087 = AXIS2_PLACEMENT_3D ( 'NONE', #6400, #62, #15282 ) ;
#11088 = CARTESIAN_POINT ( 'NONE',  ( -81.02178482187500208, -31.19062499938548427, 97.61286128772489690 ) ) ;
#11089 = CARTESIAN_POINT ( 'NONE',  ( -83.77821517812500929, -34.22812499938549280, 102.3871387122750889 ) ) ;
#11090 = DIRECTION ( 'NONE',  ( -0.000000000000000000, -1.000000000000000000, -0.000000000000000000 ) ) ;
#11091 = ORIENTED_EDGE ( 'NONE', *, *, #16886, .T. ) ;
#11092 = CARTESIAN_POINT ( 'NONE',  ( -83.90000000000000568, -33.52499999999999858, -97.40192378864668399 ) ) ;
#11093 = CARTESIAN_POINT ( 'NONE',  ( -99.99999999999998579, -29.80000000000000426, 150.0000000000000000 ) ) ;
#11094 = CARTESIAN_POINT ( 'NONE',  ( 232.3466685930879123, -34.99995246259152282, -52.98928446312130802 ) ) ;
#11095 = CARTESIAN_POINT ( 'NONE',  ( -82.40000000000001990, -32.75624999877096855, 97.00000000000000000 ) ) ;
#11096 = CARTESIAN_POINT ( 'NONE',  ( 233.9782151781249411, -30.89062499938548001, 102.3871387122750889 ) ) ;
#11097 = CARTESIAN_POINT ( 'NONE',  ( -79.39999999999999147, -34.63518749875868252, 98.26794919243110371 ) ) ;
#11098 = VERTEX_POINT ( 'NONE', #13434 ) ;
#11099 = CARTESIAN_POINT ( 'NONE',  ( -82.40000000000000568, -30.00000000000000355, 103.0000000000000000 ) ) ;
#11100 = CARTESIAN_POINT ( 'NONE',  ( 82.40000000000001990, -32.75624999877096855, -97.00000000000000000 ) ) ;
#11101 = CARTESIAN_POINT ( 'NONE',  ( -83.20384757729335945, -33.24240381056766580, 96.99999999999998579 ) ) ;
#11102 = CARTESIAN_POINT ( 'NONE',  ( 82.39999999999999147, -30.81562499938548427, 103.1828516163667899 ) ) ;
#11103 = AXIS2_PLACEMENT_3D ( 'NONE', #2355, #15357, #9787 ) ;
#11104 = FACE_BOUND ( 'NONE', #10703, .T. ) ;
#11105 = CARTESIAN_POINT ( 'NONE',  ( 85.15643035625001289, -30.25312499938548783, -99.99999999999998579 ) ) ;
#11106 = CARTESIAN_POINT ( 'NONE',  ( 229.5999999999999375, -34.91249999999999432, 101.7320508075688679 ) ) ;
#11107 = ORIENTED_EDGE ( 'NONE', *, *, #2958, .T. ) ;
#11108 = CARTESIAN_POINT ( 'NONE',  ( 83.90000000000000568, -31.81874999877096855, 102.5980762113533018 ) ) ;
#11109 = ITEM_DEFINED_TRANSFORMATION ( 'NONE', 'NONE', #6770,  #10540 ) ;
#11110 = CARTESIAN_POINT ( 'NONE',  ( 235.3564303562499447, -33.59062499938548285, 98.40857419181659793 ) ) ;
#11111 = CARTESIAN_POINT ( 'NONE',  ( 232.5999999999999375, -31.94062499938548072, -46.81714838363331666 ) ) ;
#11112 = MECHANICAL_DESIGN_GEOMETRIC_PRESENTATION_REPRESENTATION (  '', ( #17992 ), #15486 ) ;
#11113 = CARTESIAN_POINT ( 'NONE',  ( -82.39999999999999147, -33.62812499938549138, 103.1828516163667899 ) ) ;
#11114 = CARTESIAN_POINT ( 'NONE',  ( -85.15643035624999868, -35.11426555956768425, 98.99674139749697588 ) ) ;
#11115 = EDGE_LOOP ( 'NONE', ( #17116, #1939, #11107, #17498 ) ) ;
#11116 = ORIENTED_EDGE ( 'NONE', *, *, #1511, .F. ) ;
#11117 = CARTESIAN_POINT ( 'NONE',  ( -79.64356964375001269, -31.22812499938548925, -101.5914258081833879 ) ) ;
#11118 = CARTESIAN_POINT ( 'NONE',  ( -83.20384757729337366, -30.75134618820329990, 103.0000000000000000 ) ) ;
#11119 = VERTEX_POINT ( 'NONE', #3075 ) ;
#11120 = CARTESIAN_POINT ( 'NONE',  ( 79.64356964374998427, -33.21562499938548996, 98.40857419181659793 ) ) ;
#11121 = CARTESIAN_POINT ( 'NONE',  ( -82.39999999999999147, -32.75624999877096855, -103.4641016151377499 ) ) ;
#11122 = CARTESIAN_POINT ( 'NONE',  ( 94.79999999999995453, -29.80000000000000071, -150.0000000000000000 ) ) ;
#11123 = CARTESIAN_POINT ( 'NONE',  ( -82.40000000000000568, -30.00000000000000355, 103.0000000000000000 ) ) ;
#11124 = CARTESIAN_POINT ( 'NONE',  ( -85.40000000000000568, -32.19374999877096855, 99.99999999999998579 ) ) ;
#11125 = CARTESIAN_POINT ( 'NONE',  ( -85.40000000000000568, -33.13124999877096855, 98.26794919243111792 ) ) ;
#11126 = DIRECTION ( 'NONE',  ( 1.000000000000000000, -1.445602896647337931E-15, 0.000000000000000000 ) ) ;
#11127 = EDGE_CURVE ( 'NONE', #19014, #5107, #10164, .T. ) ;
#11128 = EDGE_CURVE ( 'NONE', #5078, #6543, #65, .T. ) ;
#11129 = DIRECTION ( 'NONE',  ( 0.000000000000000000, 0.000000000000000000, -1.000000000000000000 ) ) ;
#11130 = CARTESIAN_POINT ( 'NONE',  ( 230.8769377533405986, -32.00000000000000711, 102.1915028381723971 ) ) ;
#11131 = CARTESIAN_POINT ( 'NONE',  ( 233.9782151781249411, -34.79062499938547859, 97.61286128772489690 ) ) ;
#11132 = VERTEX_POINT ( 'NONE', #17751 ) ;
#11133 = CARTESIAN_POINT ( 'NONE',  ( 82.39999999999999147, -33.40312499938548285, -96.81714838363319586 ) ) ;
#11134 = CARTESIAN_POINT ( 'NONE',  ( 235.5999999999999943, -31.10624999877096286, 101.7320508075688537 ) ) ;
#11135 = CARTESIAN_POINT ( 'NONE',  ( 110.0000000000000000, 10.19999999999997620, -139.9999999999999716 ) ) ;
#11136 = VERTEX_POINT ( 'NONE', #16370 ) ;
#11137 = DIRECTION ( 'NONE',  ( -0.000000000000000000, 1.000000000000000000, -0.000000000000000000 ) ) ;
#11138 = DIRECTION ( 'NONE',  ( 1.000000000000000000, 0.000000000000000000, 0.000000000000000000 ) ) ;
#11139 = AXIS2_PLACEMENT_3D ( 'NONE', #17806, #1680, #7345 ) ;
#11140 = DIRECTION ( 'NONE',  ( 5.139921410301648824E-16, 1.000000000000000000, -3.597944987211154374E-15 ) ) ;
#11141 = VERTEX_POINT ( 'NONE', #4356 ) ;
#11142 = CARTESIAN_POINT ( 'NONE',  ( 3.961551342854190860, -3.742715940867773927, 0.5174258321190744470 ) ) ;
#11143 = EDGE_CURVE ( 'NONE', #7830, #18099, #856, .T. ) ;
#11145 = EDGE_CURVE ( 'NONE', #15108, #6865, #2886, .T. ) ;
#11144 = CARTESIAN_POINT ( 'NONE',  ( -79.39999999999999147, -33.80624999877097281, 101.7320508075688537 ) ) ;
#11146 = VERTEX_POINT ( 'NONE', #1425 ) ;
#11147 = DIRECTION ( 'NONE',  ( 1.000000000000000000, -0.000000000000000000, -0.000000000000000000 ) ) ;
#11148 = CARTESIAN_POINT ( 'NONE',  ( 83.77821517812500929, -34.56562499938548427, -102.3871387122750889 ) ) ;
#11149 = CARTESIAN_POINT ( 'NONE',  ( -4.000000000000000000, -2.309401076758515803, -0.4999999999999995559 ) ) ;
#11150 = VECTOR ( 'NONE', #11972, 1000.000000000000000 ) ;
#11151 =( GEOMETRIC_REPRESENTATION_CONTEXT ( 3 ) GLOBAL_UNCERTAINTY_ASSIGNED_CONTEXT ( ( #3353 ) ) GLOBAL_UNIT_ASSIGNED_CONTEXT ( ( #9798, #14090, #2850 ) ) REPRESENTATION_CONTEXT ( 'NONE', 'WORKASPACE' ) );
#11152 = CARTESIAN_POINT ( 'NONE',  ( -83.90000000000000568, -34.81874999877096855, 102.5980762113533018 ) ) ;
#11153 = CARTESIAN_POINT ( 'NONE',  ( -79.39999999999999147, -30.22500000000000142, 99.99999999999998579 ) ) ;
#11154 = DIRECTION ( 'NONE',  ( -0.000000000000000000, -1.000000000000000000, -0.000000000000000000 ) ) ;
#11155 = SURFACE_SIDE_STYLE ('',( #18592 ) ) ;
#11156 = EDGE_CURVE ( 'NONE', #11820, #5897, #18041, .T. ) ;
#11157 = CARTESIAN_POINT ( 'NONE',  ( 79.64356964374998427, -32.20312499938548711, 98.40857419181659793 ) ) ;
#11158 = CARTESIAN_POINT ( 'NONE',  ( -79.39999999999999147, -33.80624999877097281, 101.7320508075688537 ) ) ;
#11159 = CARTESIAN_POINT ( 'NONE',  ( -79.64356964374999848, -33.51562499938548711, 99.99999999999998579 ) ) ;
#11160 = CARTESIAN_POINT ( 'NONE',  ( 246.9999999999999716, -5.000000000000004441, -100.0000000000000000 ) ) ;
#11161 = ORIENTED_EDGE ( 'NONE', *, *, #6147, .T. ) ;
#11162 =( BOUNDED_CURVE ( )  B_SPLINE_CURVE ( 2, ( #2368, #11458, #16144, #2757, #14666, #10090, #1202, #18989, #9899 ),
 .UNSPECIFIED., .F., .F. ) 
 B_SPLINE_CURVE_WITH_KNOTS ( ( 3, 2, 2, 2, 3 ),
 ( 0.5208333333333333703, 0.5277777777777777901, 0.5416666666666666297, 0.5555555555555555802, 0.5625000000000000000 ),
 .UNSPECIFIED. ) 
 CURVE ( )  GEOMETRIC_REPRESENTATION_ITEM ( )  RATIONAL_B_SPLINE_CURVE ( ( 0.9330127018922192983, 0.9330127018922198534, 1.000000000000000000, 0.8660254037844387076, 1.000000000000000000, 0.8660254037844387076, 1.000000000000000000, 0.9330127018922194093, 0.9330127018922194093 ) ) 
 REPRESENTATION_ITEM ( '' )  );
#11163 = CARTESIAN_POINT ( 'NONE',  ( 229.5999999999999375, -34.08749999999999147, -51.73205080756898866 ) ) ;
#11164 = CARTESIAN_POINT ( 'NONE',  ( -83.90000000000000568, -33.52499999999999858, 102.5980762113533018 ) ) ;
#11165 = AXIS2_PLACEMENT_3D ( 'NONE', #18155, #382, #477 ) ;
#11166 = B_SPLINE_CURVE_WITH_KNOTS ( 'NONE', 3,
 ( #17604, #17511, #6964, #11734, #14462, #15857 ),
 .UNSPECIFIED., .F., .F.,
 ( 4, 2, 4 ),
 ( 0.002044882221487525839, 0.003063384235218491979, 0.004081886248949458118 ),
 .UNSPECIFIED. ) ;
#11167 = DIRECTION ( 'NONE',  ( 0.000000000000000000, 0.000000000000000000, 1.000000000000000000 ) ) ;
#11168 = CARTESIAN_POINT ( 'NONE',  ( 232.5999999999999943, -32.61562499938548143, 96.81714838363319586 ) ) ;
#11169 = CARTESIAN_POINT ( 'NONE',  ( -83.77821517812500929, -33.77812499938548285, 102.3871387122750889 ) ) ;
#11170 = CARTESIAN_POINT ( 'NONE',  ( 231.2217848218749339, -31.41562499938547859, -47.61286128772501769 ) ) ;
#11171 = ORIENTED_EDGE ( 'NONE', *, *, #7224, .T. ) ;
#11172 = CARTESIAN_POINT ( 'NONE',  ( 3.972058292797709278, 0.6948821373597366957, 3.565770528409240470 ) ) ;
#11173 = CIRCLE ( 'NONE', #5882, 2.500000000000000444 ) ;
#11174 = CARTESIAN_POINT ( 'NONE',  ( 81.96801452314024061, -34.99999999999999289, 97.27181766474434710 ) ) ;
#11175 = CARTESIAN_POINT ( 'NONE',  ( 79.64356964375001269, -32.57812499938548001, 101.5914258081833879 ) ) ;
#11176 = CARTESIAN_POINT ( 'NONE',  ( -0.5636800770129166693, -4.293361309317430319, -3.531542292955206275 ) ) ;
#11177 = AXIS2_PLACEMENT_3D ( 'NONE', #9544, #7694, #6623 ) ;
#11178 = VECTOR ( 'NONE', #12794, 1000.000000000000000 ) ;
#11179 = CARTESIAN_POINT ( 'NONE',  ( 82.39999999999999147, -32.58749999999999858, 96.99999999999998579 ) ) ;
#11180 = CARTESIAN_POINT ( 'NONE',  ( -81.02178482187500208, -34.00312499938548427, 97.61286128772489690 ) ) ;
#11181 = CARTESIAN_POINT ( 'NONE',  ( 230.2961164517930968, -35.00002705695778360, 98.07851859032987818 ) ) ;
#11182 = CARTESIAN_POINT ( 'NONE',  ( 79.64356964375001269, -31.67812499938548143, 101.5914258081833879 ) ) ;
#11183 = CARTESIAN_POINT ( 'NONE',  ( 82.39999999999999147, -34.41562499938547859, -96.81714838363319586 ) ) ;
#11184 = EDGE_CURVE ( 'NONE', #592, #11539, #11967, .T. ) ;
#11185 = CARTESIAN_POINT ( 'NONE',  ( 233.9782151781249411, -33.59062499938547575, -47.61286128772501769 ) ) ;
#11186 = CARTESIAN_POINT ( 'NONE',  ( -79.64356964374998427, -33.59062499938548285, 98.40857419181659793 ) ) ;
#11187 = CARTESIAN_POINT ( 'NONE',  ( -85.15643035624999868, -31.52812499938547930, -101.5914258081833879 ) ) ;
#11188 = ORIENTED_EDGE ( 'NONE', *, *, #11525, .F. ) ;
#11189 = CARTESIAN_POINT ( 'NONE',  ( 81.02178482187500208, -33.55312499938548854, 102.3871387122750889 ) ) ;
#11190 = CARTESIAN_POINT ( 'NONE',  ( 232.5999999999999375, -32.75624999877096144, 96.99999999999998579 ) ) ;
#11191 = CARTESIAN_POINT ( 'NONE',  ( -82.39999999999999147, -33.03750000000000142, 103.4641016151377499 ) ) ;
#11192 = CARTESIAN_POINT ( 'NONE',  ( -85.15643035625001289, -31.94062499938548427, 99.99999999999998579 ) ) ;
#11193 = CARTESIAN_POINT ( 'NONE',  ( -82.39999999999999147, -34.64062499938548711, 103.1828516163667899 ) ) ;
#11194 = CARTESIAN_POINT ( 'NONE',  ( 82.40000000000001990, -32.75624999877096855, -97.00000000000000000 ) ) ;
#11195 = ORIENTED_EDGE ( 'NONE', *, *, #3753, .T. ) ;
#11196 = CARTESIAN_POINT ( 'NONE',  ( -82.39999999999999147, -34.61250000000000426, -103.4641016151377499 ) ) ;
#11197 = CARTESIAN_POINT ( 'NONE',  ( 81.59615242270662350, -33.01740381056767148, -102.9999999999999858 ) ) ;
#11198 = CARTESIAN_POINT ( 'NONE',  ( 230.4285530052381716, -35.00000000000000000, -52.07926958674877937 ) ) ;
#11199 = CARTESIAN_POINT ( 'NONE',  ( -80.90000000000000568, -30.59606250001229100, 97.40192378864668399 ) ) ;
#11200 = CARTESIAN_POINT ( 'NONE',  ( 232.5999999999999375, -31.60312499938548214, 96.81714838363319586 ) ) ;
#11201 = CARTESIAN_POINT ( 'NONE',  ( -85.40000000000000568, -35.34768749875867400, 99.99999999999998579 ) ) ;
#11202 = EDGE_CURVE ( 'NONE', #1356, #10773, #10503, .T. ) ;
#11203 = APPLICATION_CONTEXT ( 'automotive_design' ) ;
#11204 = CARTESIAN_POINT ( 'NONE',  ( -82.65333140691201663, -34.99995246259153703, 97.01071553687880566 ) ) ;
#11205 = CARTESIAN_POINT ( 'NONE',  ( 233.4038475772933339, -32.83259618943232994, 96.99999999999998579 ) ) ;
#11206 = DIRECTION ( 'NONE',  ( 0.000000000000000000, 0.000000000000000000, 1.000000000000000000 ) ) ;
#11207 = CARTESIAN_POINT ( 'NONE',  ( 82.39999999999999147, -30.59062499938548640, 96.81714838363319586 ) ) ;
#11208 = CARTESIAN_POINT ( 'NONE',  ( 8.673617379884035472E-16, 4.618802153517012954, 0.000000000000000000 ) ) ;
#11209 = PLANE ( 'NONE',  #2769 ) ;
#11210 = CARTESIAN_POINT ( 'NONE',  ( 85.15643035625001289, -31.60312499938548569, -99.99999999999998579 ) ) ;
#11211 = FACE_BOUND ( 'NONE', #9362, .T. ) ;
#11212 = VERTEX_POINT ( 'NONE', #4547 ) ;
#11213 = CARTESIAN_POINT ( 'NONE',  ( 79.39999999999999147, -31.93124999877096926, 101.7320508075688821 ) ) ;
#11214 = SHAPE_DEFINITION_REPRESENTATION ( #3575, #9634 ) ;
#11215 = CARTESIAN_POINT ( 'NONE',  ( 229.8435696437499871, -31.56562499938547717, 101.5914258081833879 ) ) ;
#11216 = CARTESIAN_POINT ( 'NONE',  ( 235.3564303562499447, -32.27812499938548285, -50.00000000000011369 ) ) ;
#11217 = CARTESIAN_POINT ( 'NONE',  ( -82.39999999999999147, -33.17812499938548854, 103.1828516163667899 ) ) ;
#11218 = CARTESIAN_POINT ( 'NONE',  ( 83.20384757729338787, -33.95759618943233704, 97.00000000000000000 ) ) ;
#11219 = VERTEX_POINT ( 'NONE', #16470 ) ;
#11220 = CARTESIAN_POINT ( 'NONE',  ( -82.39999999999999147, -31.60312499938548569, -103.1828516163667899 ) ) ;
#11221 = CARTESIAN_POINT ( 'NONE',  ( 99.99999999999997158, -5.200000000000008171, 150.0000000000000000 ) ) ;
#11222 = EDGE_LOOP ( 'NONE', ( #707, #14149, #5386, #8398 ) ) ;
#11223 = CARTESIAN_POINT ( 'NONE',  ( 81.02178482187500208, -34.00312499938548427, 102.3871387122750889 ) ) ;
#11224 = CARTESIAN_POINT ( 'NONE',  ( -83.90000000000000568, -32.71874999877096712, -102.5980762113533018 ) ) ;
#11225 = CARTESIAN_POINT ( 'NONE',  ( 80.90000000000000568, -34.20000000000000284, 102.5980762113533018 ) ) ;
#11226 = CARTESIAN_POINT ( 'NONE',  ( -79.91954014136210560, -34.99999999999999289, 98.55723758691019043 ) ) ;
#11227 = CARTESIAN_POINT ( 'NONE',  ( -80.90000000000000568, -31.44374999877096855, 97.40192378864668399 ) ) ;
#11228 = CARTESIAN_POINT ( 'NONE',  ( -79.39999999999999147, -32.83124999877097139, 98.26794919243110371 ) ) ;
#11229 = CARTESIAN_POINT ( 'NONE',  ( 84.85538848573307291, -35.00000000000139977, -98.27756861396950683 ) ) ;
#11230 =( BOUNDED_CURVE ( )  B_SPLINE_CURVE ( 2, ( #7624, #14681, #19191, #10105, #1858, #319, #6360, #4241, #13218 ),
 .UNSPECIFIED., .F., .F. ) 
 B_SPLINE_CURVE_WITH_KNOTS ( ( 3, 2, 2, 2, 3 ),
 ( 0.1041666666666666713, 0.1111111111111111049, 0.1250000000000000000, 0.1388888888888888951, 0.1458333333333333426 ),
 .UNSPECIFIED. ) 
 CURVE ( )  GEOMETRIC_REPRESENTATION_ITEM ( )  RATIONAL_B_SPLINE_CURVE ( ( 0.9330127018922194093, 0.9330127018922194093, 1.000000000000000000, 0.8660254037844387076, 1.000000000000000000, 0.8660254037844387076, 1.000000000000000000, 0.9330127018922194093, 0.9330127018922194093 ) ) 
 REPRESENTATION_ITEM ( '' )  );
#11231 = PRODUCT_DEFINITION_SHAPE ( 'NONE', 'NONE',  #19330 ) ;
#11232 = CARTESIAN_POINT ( 'NONE',  ( 231.7961524227065411, -34.08615380933862582, -53.00000000000009237 ) ) ;
#11233 = DIRECTION ( 'NONE',  ( -1.000000000000000000, 0.000000000000000000, 0.000000000000000000 ) ) ;
#11234 = CARTESIAN_POINT ( 'NONE',  ( 235.3564303562499447, -33.92812499938548143, 98.40857419181659793 ) ) ;
#11235 = ORIENTED_EDGE ( 'NONE', *, *, #5596, .F. ) ;
#11236 = CARTESIAN_POINT ( 'NONE',  ( 85.15643035625001289, -32.35312499938548569, -101.5914258081833879 ) ) ;
#11237 = CARTESIAN_POINT ( 'NONE',  ( 229.5999999999999375, -30.43124999877096215, 98.26794919243111792 ) ) ;
#11238 = CARTESIAN_POINT ( 'NONE',  ( 232.5999999999999375, -31.85624999877096641, -53.46410161513786363 ) ) ;
#11239 = ORIENTED_EDGE ( 'NONE', *, *, #6417, .F. ) ;
#11240 = CARTESIAN_POINT ( 'NONE',  ( 232.5999999999999375, -32.75624999877096144, 96.99999999999998579 ) ) ;
#11241 = CARTESIAN_POINT ( 'NONE',  ( -85.15643035625001289, -30.17812499938548498, 98.40857419181659793 ) ) ;
#11242 = DIRECTION ( 'NONE',  ( 0.000000000000000000, 0.000000000000000000, -1.000000000000000000 ) ) ;
#11243 = ORIENTED_EDGE ( 'NONE', *, *, #16274, .T. ) ;
#11244 = CARTESIAN_POINT ( 'NONE',  ( -83.90000000000000568, -33.91874999877096997, -97.40192378864668399 ) ) ;
#11245 = CARTESIAN_POINT ( 'NONE',  ( 233.4038475772933339, -33.67634618820329706, -53.00000000000011369 ) ) ;
#11246 = ORIENTED_EDGE ( 'NONE', *, *, #187, .F. ) ;
#11247 = SURFACE_STYLE_USAGE ( .BOTH. , #2257 ) ;
#11248 = CARTESIAN_POINT ( 'NONE',  ( 79.39999999999999147, -31.61250000000000071, -101.7320508075688537 ) ) ;
#11249 = CARTESIAN_POINT ( 'NONE',  ( 4.050536630291690976, -2.401306687817041929, 2.976670123173769333 ) ) ;
#11250 = CARTESIAN_POINT ( 'NONE',  ( -81.02178482187500208, -31.90312499938548996, 102.3871387122750889 ) ) ;
#11251 = CARTESIAN_POINT ( 'NONE',  ( -79.39999999999999147, -33.78356250001230165, 98.26794919243110371 ) ) ;
#11252 = CARTESIAN_POINT ( 'NONE',  ( -5.560781378645573980, 0.000000000000000000, -4.000000000000000000 ) ) ;
#11253 = CARTESIAN_POINT ( 'NONE',  ( 232.5999999999999375, -29.99999999999999645, -50.00000000000011369 ) ) ;
#11254 = CARTESIAN_POINT ( 'NONE',  ( 79.64356964374998427, -34.94062499938548427, -98.40857419181659793 ) ) ;
#11255 = CARTESIAN_POINT ( 'NONE',  ( -82.40000000000000568, -30.00000000000000355, 99.99999999999998579 ) ) ;
#11256 = CARTESIAN_POINT ( 'NONE',  ( -82.39999999999999147, -32.95312499938548711, 96.81714838363319586 ) ) ;
#11257 = DIRECTION ( 'NONE',  ( 0.000000000000000000, 1.000000000000000000, 0.000000000000000000 ) ) ;
#11258 = EDGE_LOOP ( 'NONE', ( #1496, #7833, #9237, #222, #10446, #18050, #9101, #10854, #3545, #17921, #14687, #1595, #4152, #5468, #4461, #12278, #3024, #17259, #9138, #18008, #7509, #9843, #15353, #12444, #8978, #7299 ) ) ;
#11259 =( NAMED_UNIT ( * ) SI_UNIT ( $, .STERADIAN. ) SOLID_ANGLE_UNIT ( ) );
#11260 = DIRECTION ( 'NONE',  ( 0.000000000000000000, -1.000000000000000000, 0.000000000000000000 ) ) ;
#11261 = CARTESIAN_POINT ( 'NONE',  ( 229.5999999999999375, -34.94999999999999574, -50.00000000000011369 ) ) ;
#11262 = CARTESIAN_POINT ( 'NONE',  ( -85.15643035624999868, -33.89062499938548711, 98.40857419181659793 ) ) ;
#11263 = CARTESIAN_POINT ( 'NONE',  ( 231.2217848218749339, -30.66562499938547859, -52.38713871227520968 ) ) ;
#11264 = EDGE_CURVE ( 'NONE', #13128, #18799, #16047, .T. ) ;
#11265 = ORIENTED_EDGE ( 'NONE', *, *, #11558, .T. ) ;
#11266 = CARTESIAN_POINT ( 'NONE',  ( -81.28488860390726245, -34.99999999999999289, -97.47285052570516939 ) ) ;
#11267 = CARTESIAN_POINT ( 'NONE',  ( -83.77821517812500929, -35.01562499938548711, 102.3871387122750889 ) ) ;
#11268 = CARTESIAN_POINT ( 'NONE',  ( 79.64356964375001269, -31.67812499938548143, 101.5914258081833879 ) ) ;
#11269 = CARTESIAN_POINT ( 'NONE',  ( -82.39999999999999147, -31.46249999999999858, 96.99999999999998579 ) ) ;
#11270 = DIRECTION ( 'NONE',  ( 0.000000000000000000, 1.000000000000000000, 0.000000000000000000 ) ) ;
#11271 =( BOUNDED_CURVE ( )  B_SPLINE_CURVE ( 2, ( #10470, #11557, #16247, #17520, #7162, #10093, #16051, #2654, #19081 ),
 .UNSPECIFIED., .F., .F. ) 
 B_SPLINE_CURVE_WITH_KNOTS ( ( 3, 2, 2, 2, 3 ),
 ( 0.4375000000000000555, 0.4444444444444444198, 0.4583333333333333148, 0.4722222222222222099, 0.4791666666666666297 ),
 .UNSPECIFIED. ) 
 CURVE ( )  GEOMETRIC_REPRESENTATION_ITEM ( )  RATIONAL_B_SPLINE_CURVE ( ( 0.9330127018922192983, 0.9330127018922198534, 1.000000000000000000, 0.8660254037844387076, 1.000000000000000000, 0.8660254037844387076, 1.000000000000000000, 0.9330127018922196314, 0.9330127018922194093 ) ) 
 REPRESENTATION_ITEM ( '' )  );
#11272 = EDGE_CURVE ( 'NONE', #8694, #13696, #18817, .T. ) ;
#11273 = CARTESIAN_POINT ( 'NONE',  ( -85.15643035625001289, -33.85312499938549280, 99.99999999999998579 ) ) ;
#11274 = CARTESIAN_POINT ( 'NONE',  ( -81.02178482187500208, -34.15312499938548285, -97.61286128772489690 ) ) ;
#11275 = CARTESIAN_POINT ( 'NONE',  ( 83.77821517812500929, -33.21562499938548285, 97.61286128772489690 ) ) ;
#11276 = EDGE_CURVE ( 'NONE', #3690, #867, #17633, .T. ) ;
#11277 = CARTESIAN_POINT ( 'NONE',  ( 85.15643035624999868, -32.99062499938548854, -98.40857419181659793 ) ) ;
#11278 = CARTESIAN_POINT ( 'NONE',  ( 229.8435696437499871, -33.77812499938548285, -51.59142580818350865 ) ) ;
#11279 = CARTESIAN_POINT ( 'NONE',  ( -85.15643035625001289, -32.80312499938548854, 101.5914258081833879 ) ) ;
#11280 = CARTESIAN_POINT ( 'NONE',  ( 82.39999999999999147, -30.70312499938548711, -96.81714838363319586 ) ) ;
#11281 = EDGE_CURVE ( 'NONE', #4201, #779, #18056, .T. ) ;
#11282 = VERTEX_POINT ( 'NONE', #11179 ) ;
#11283 = CARTESIAN_POINT ( 'NONE',  ( 79.64356964374999848, -32.72812499938548569, 99.99999999999998579 ) ) ;
#11284 = FACE_OUTER_BOUND ( 'NONE', #3090, .T. ) ;
#11285 = CARTESIAN_POINT ( 'NONE',  ( -85.40000000000000568, -34.08749999999999858, 98.26794919243111792 ) ) ;
#11286 = CARTESIAN_POINT ( 'NONE',  ( -81.02178482187500208, -30.74062499938548498, 97.61286128772489690 ) ) ;
#11287 = CARTESIAN_POINT ( 'NONE',  ( -79.64356964375001269, -30.32812499938548711, 98.40857419181659793 ) ) ;
#11288 = FACE_OUTER_BOUND ( 'NONE', #15554, .T. ) ;
#11289 = ORIENTED_EDGE ( 'NONE', *, *, #10666, .T. ) ;
#11290 = CARTESIAN_POINT ( 'NONE',  ( -82.39999999999999147, -32.36250000000000426, -103.4641016151377499 ) ) ;
#11291 = AXIS2_PLACEMENT_3D ( 'NONE', #4085, #5372, #14524 ) ;
#11292 = AXIS2_PLACEMENT_3D ( 'NONE', #11841, #14669, #1304 ) ;
#11293 = CYLINDRICAL_SURFACE ( 'NONE', #11919, 3.000000000000002665 ) ;
#11294 = CARTESIAN_POINT ( 'NONE',  ( 229.5999999999999375, -34.08749999999999147, -51.73205080756898866 ) ) ;
#11295 = EDGE_CURVE ( 'NONE', #19282, #16293, #16834, .T. ) ;
#11296 = CARTESIAN_POINT ( 'NONE',  ( 83.90000000000000568, -33.52499999999999858, -102.5980762113533018 ) ) ;
#11297 = CARTESIAN_POINT ( 'NONE',  ( 4.180231891692620216, 4.134807952925571684, 0.02076457676760292553 ) ) ;
#11298 = CARTESIAN_POINT ( 'NONE',  ( 85.40000000000000568, -34.03124999877096712, -98.26794919243111792 ) ) ;
#11299 = CARTESIAN_POINT ( 'NONE',  ( 232.5999999999999375, -29.99999999999999645, 96.99999999999998579 ) ) ;
#11300 = CARTESIAN_POINT ( 'NONE',  ( 229.8306817459157401, -31.99999999999999289, 100.2387112178437150 ) ) ;
#11301 = CARTESIAN_POINT ( 'NONE',  ( 79.64356964375001269, -31.34062499938548640, 101.5914258081833879 ) ) ;
#11302 = DIRECTION ( 'NONE',  ( -0.000000000000000000, -1.000000000000000000, -0.000000000000000000 ) ) ;
#11303 = CARTESIAN_POINT ( 'NONE',  ( -83.90000000000000568, -32.62500000000000000, -97.40192378864668399 ) ) ;
#11304 = CARTESIAN_POINT ( 'NONE',  ( 79.64356964375001269, -32.24062499938548854, -98.40857419181659793 ) ) ;
#11305 = CARTESIAN_POINT ( 'NONE',  ( 4.175572532730931208, 2.061029303918050726, 3.569807470274392713 ) ) ;
#11306 = CIRCLE ( 'NONE', #4445, 3.000000000000002665 ) ;
#11307 = CONICAL_SURFACE ( 'NONE', #13796, 3.500000000000000000, 1.047197551196600296 ) ;
#11308 =( BOUNDED_CURVE ( )  B_SPLINE_CURVE ( 2, ( #8151, #14103, #3458, #739, #13719, #15383, #2478, #14481, #3845 ),
 .UNSPECIFIED., .F., .F. ) 
 B_SPLINE_CURVE_WITH_KNOTS ( ( 3, 2, 2, 2, 3 ),
 ( 0.3958333333333334259, 0.4027777777777777901, 0.4166666666666666852, 0.4305555555555555802, 0.4374999999999999445 ),
 .UNSPECIFIED. ) 
 CURVE ( )  GEOMETRIC_REPRESENTATION_ITEM ( )  RATIONAL_B_SPLINE_CURVE ( ( 0.9330127018922192983, 0.9330127018922200755, 1.000000000000000000, 0.8660254037844387076, 1.000000000000000000, 0.8660254037844387076, 1.000000000000000000, 0.9330127018922198534, 0.9330127018922192983 ) ) 
 REPRESENTATION_ITEM ( '' )  );
#11309 = ORIENTED_EDGE ( 'NONE', *, *, #14586, .F. ) ;
#11310 = CARTESIAN_POINT ( 'NONE',  ( 82.39999999999999147, -30.95624999877097139, 103.4641016151377499 ) ) ;
#11311 = ITEM_DEFINED_TRANSFORMATION ( 'NONE', 'NONE', #5813,  #10540 ) ;
#11312 = CARTESIAN_POINT ( 'NONE',  ( 229.8435696437499871, -35.22676544108146857, 98.99674642581742035 ) ) ;
#11313 = EDGE_CURVE ( 'NONE', #16053, #13878, #7151, .T. ) ;
#11314 = CARTESIAN_POINT ( 'NONE',  ( 231.2217848218749339, -34.22812499938548569, -47.61286128772501769 ) ) ;
#11315 = CARTESIAN_POINT ( 'NONE',  ( -85.15643035624999868, -30.29062499938548925, 98.40857419181659793 ) ) ;
#11316 = PLANE ( 'NONE',  #5256 ) ;
#11317 = ORIENTED_EDGE ( 'NONE', *, *, #1293, .T. ) ;
#11318 = CARTESIAN_POINT ( 'NONE',  ( -85.15643035624999868, -32.80312499938548854, -98.40857419181659793 ) ) ;
#11319 = CARTESIAN_POINT ( 'NONE',  ( 83.20384757729335945, -33.24240381056766580, 102.9999999999999716 ) ) ;
#11320 = ORIENTED_EDGE ( 'NONE', *, *, #13166, .F. ) ;
#11321 = CARTESIAN_POINT ( 'NONE',  ( 83.77821517812500929, -34.67812499938548854, 97.61286128772489690 ) ) ;
#11322 = ADVANCED_FACE ( 'NONE', ( #10886 ), #10466, .F. ) ;
#11323 = CARTESIAN_POINT ( 'NONE',  ( -79.64356964375001269, -30.89062499938548711, -101.5914258081833879 ) ) ;
#11324 = CARTESIAN_POINT ( 'NONE',  ( 85.40000000000000568, -34.95000000000000284, 99.99999999999998579 ) ) ;
#11325 = CARTESIAN_POINT ( 'NONE',  ( -80.32125193361312654, -35.00000000000000711, 97.97655282300750912 ) ) ;
#11326 = CARTESIAN_POINT ( 'NONE',  ( -79.39999999999999147, -34.18124999877097281, 98.26794919243110371 ) ) ;
#11327 = CARTESIAN_POINT ( 'NONE',  ( -83.77821517812500929, -31.97812499938548925, 102.3871387122750889 ) ) ;
#11328 = DIRECTION ( 'NONE',  ( -1.000000000000000000, 0.000000000000000000, 0.000000000000000000 ) ) ;
#11329 = DIRECTION ( 'NONE',  ( 0.000000000000000000, 0.000000000000000000, -1.000000000000000000 ) ) ;
#11330 = CARTESIAN_POINT ( 'NONE',  ( 105.1999999999999886, -29.80000000000001492, -97.80000000000002558 ) ) ;
#11331 = CARTESIAN_POINT ( 'NONE',  ( 231.0999999999999375, -31.72499999999999787, 102.5980762113533018 ) ) ;
#11332 = EDGE_LOOP ( 'NONE', ( #11340, #7114, #3468, #942 ) ) ;
#11333 = CARTESIAN_POINT ( 'NONE',  ( 79.64356964374998427, -33.10312499938548569, -101.5914258081833879 ) ) ;
#11334 = CARTESIAN_POINT ( 'NONE',  ( 229.5999999999999375, -33.95624999877095718, 101.7320508075688679 ) ) ;
#11335 = CARTESIAN_POINT ( 'NONE',  ( 229.5999999999999375, -32.23124999877096286, -51.73205080756898866 ) ) ;
#11336 = ORIENTED_EDGE ( 'NONE', *, *, #8993, .T. ) ;
#11337 = CARTESIAN_POINT ( 'NONE',  ( 83.20384757729335945, -32.60759618943233562, 96.99999999999997158 ) ) ;
#11338 = CARTESIAN_POINT ( 'NONE',  ( -85.15643035625001289, -31.52812499938548285, 98.40857419181659793 ) ) ;
#11339 = DIRECTION ( 'NONE',  ( 1.000000000000000000, 0.000000000000000000, 0.000000000000000000 ) ) ;
#11340 = ORIENTED_EDGE ( 'NONE', *, *, #11202, .F. ) ;
#11341 = FACE_OUTER_BOUND ( 'NONE', #13224, .T. ) ;
#11342 = CARTESIAN_POINT ( 'NONE',  ( 231.7961524227065979, -33.18615380933862724, 97.00000000000000000 ) ) ;
#11343 = ORIENTED_EDGE ( 'NONE', *, *, #9244, .T. ) ;
#11344 = CARTESIAN_POINT ( 'NONE',  ( -79.39999999999999147, -32.06250000000000000, -98.26794919243113213 ) ) ;
#11345 = CARTESIAN_POINT ( 'NONE',  ( 79.39999999999999147, -33.33749999999999858, -98.26794919243110371 ) ) ;
#11346 = CARTESIAN_POINT ( 'NONE',  ( 235.3140393761304665, -32.00000000000000000, -48.72172371342785624 ) ) ;
#11347 =( BOUNDED_CURVE ( )  B_SPLINE_CURVE ( 2, ( #9473, #4998, #1953, #8007, #13966, #698, #9674, #11232, #2048 ),
 .UNSPECIFIED., .F., .F. ) 
 B_SPLINE_CURVE_WITH_KNOTS ( ( 3, 2, 2, 2, 3 ),
 ( 0.6458333333333331483, 0.6527777777777777901, 0.6666666666666666297, 0.6805555555555555802, 0.6874999999999997780 ),
 .UNSPECIFIED. ) 
 CURVE ( )  GEOMETRIC_REPRESENTATION_ITEM ( )  RATIONAL_B_SPLINE_CURVE ( ( 0.9330127018922194093, 0.9330127018922177440, 1.000000000000000000, 0.8660254037844387076, 1.000000000000000000, 0.8660254037844387076, 1.000000000000000000, 0.9330127018922215187, 0.9330127018922194093 ) ) 
 REPRESENTATION_ITEM ( '' )  );
#11348 = CARTESIAN_POINT ( 'NONE',  ( -82.39999999999999147, -32.61562499938548854, 96.81714838363319586 ) ) ;
#11349 = CARTESIAN_POINT ( 'NONE',  ( -85.40000000000000568, -29.95670094768209779, 101.9998975609119469 ) ) ;
#11350 = LINE ( 'NONE', #13194, #4940 ) ;
#11351 = CARTESIAN_POINT ( 'NONE',  ( 234.1999394931801532, -31.99999999999997868, -52.45377063617920754 ) ) ;
#11352 = CARTESIAN_POINT ( 'NONE',  ( 85.15643035625001289, -34.34062499938548285, -98.40857419181659793 ) ) ;
#11353 = CARTESIAN_POINT ( 'NONE',  ( -81.59615242270665192, -33.86115380933864571, 103.0000000000000000 ) ) ;
#11354 = CARTESIAN_POINT ( 'NONE',  ( 85.31192385480825635, -35.00000000000000711, 100.3932545473399642 ) ) ;
#11355 = FACE_BOUND ( 'NONE', #15638, .T. ) ;
#11356 = ORIENTED_EDGE ( 'NONE', *, *, #9427, .T. ) ;
#11357 = DIRECTION ( 'NONE',  ( -0.000000000000000000, -1.000000000000000000, -0.000000000000000000 ) ) ;
#11358 = CARTESIAN_POINT ( 'NONE',  ( 233.9419434205216533, -34.99999999999999289, 97.38506107425222069 ) ) ;
#11359 = CARTESIAN_POINT ( 'NONE',  ( -84.70388354820684640, -35.00002705695768412, -101.9214814096701076 ) ) ;
#11360 = CARTESIAN_POINT ( 'NONE',  ( 231.2217848218749339, -34.67812499938548143, 102.3871387122750889 ) ) ;
#11361 = CARTESIAN_POINT ( 'NONE',  ( -81.02178482187500208, -33.10312499938548569, 97.61286128772489690 ) ) ;
#11362 = CARTESIAN_POINT ( 'NONE',  ( 232.5999999999999375, -35.09062499938547575, -46.81714838363331666 ) ) ;
#11363 = VERTEX_POINT ( 'NONE', #3656 ) ;
#11364 = CARTESIAN_POINT ( 'NONE',  ( -80.17984880387896851, -35.00000000000000000, -98.35655086105390410 ) ) ;
#11365 = CARTESIAN_POINT ( 'NONE',  ( -82.39999999999999147, -32.95312499938548711, 96.81714838363319586 ) ) ;
#11366 = DIRECTION ( 'NONE',  ( 1.000000000000000000, 0.000000000000000000, 0.000000000000000000 ) ) ;
#11367 = CARTESIAN_POINT ( 'NONE',  ( 82.39999999999999147, -33.85312499938547859, 103.1828516163667899 ) ) ;
#11368 = CARTESIAN_POINT ( 'NONE',  ( 83.20384757729338787, -33.95759618943233704, -102.9999999999999858 ) ) ;
#11369 = CARTESIAN_POINT ( 'NONE',  ( -82.40000000000000568, -30.00000000000000355, -99.99999999999998579 ) ) ;
#11370 = CARTESIAN_POINT ( 'NONE',  ( -79.64356964374999848, -32.72812499938548569, 99.99999999999998579 ) ) ;
#11371 = CARTESIAN_POINT ( 'NONE',  ( -79.64356964374999848, -34.52812499938548285, -99.99999999999998579 ) ) ;
#11372 = CARTESIAN_POINT ( 'NONE',  ( 85.15643035624999868, -32.87812499938549138, 101.5914258081833879 ) ) ;
#11373 = EDGE_CURVE ( 'NONE', #10346, #5045, #11308, .T. ) ;
#11374 = EDGE_CURVE ( 'NONE', #17568, #8145, #17241, .T. ) ;
#11375 = CARTESIAN_POINT ( 'NONE',  ( 83.77821517812500929, -34.82812499938548711, -97.61286128772489690 ) ) ;
#11376 = CARTESIAN_POINT ( 'NONE',  ( 229.8435696437499871, -33.32812499938548001, -51.59142580818350865 ) ) ;
#11377 = CARTESIAN_POINT ( 'NONE',  ( -83.77821517812500929, -34.26562499938548711, 97.61286128772489690 ) ) ;
#11378 = CARTESIAN_POINT ( 'NONE',  ( 85.15643035625001289, -30.14062499938548711, -99.99999999999998579 ) ) ;
#11379 = VERTEX_POINT ( 'NONE', #11470 ) ;
#11380 = CARTESIAN_POINT ( 'NONE',  ( 110.0000000000000142, 10.19999999999995666, 50.00000000000001421 ) ) ;
#11381 = CARTESIAN_POINT ( 'NONE',  ( 1.360585162435110629, -4.061296242128317857, -3.505054077164905024 ) ) ;
#11382 = CARTESIAN_POINT ( 'NONE',  ( -85.40000000000000568, -33.56250000000000000, 101.7320508075688679 ) ) ;
#11383 = CARTESIAN_POINT ( 'NONE',  ( -79.64356964375001269, -33.92812499938548854, 98.40857419181659793 ) ) ;
#11384 = CARTESIAN_POINT ( 'NONE',  ( -82.39999999999999147, -31.60312499938548569, 96.81714838363319586 ) ) ;
#11385 = CARTESIAN_POINT ( 'NONE',  ( -82.40000000000000568, -30.00000000000000355, 103.0000000000000000 ) ) ;
#11386 = CARTESIAN_POINT ( 'NONE',  ( -84.82992844608097016, -31.99999999999998579, 98.68659295968647882 ) ) ;
#11387 = CIRCLE ( 'NONE', #11075, 7.500000000000020428 ) ;
#11388 = PRODUCT ( 'hex flange bolt small_iso_ISO 4162 - M5 x 20 x 20-N', 'hex flange bolt small_iso_ISO 4162 - M5 x 20 x 20-N', '', ( #14045 ) ) ;
#11389 = EDGE_CURVE ( 'NONE', #13275, #5463, #12839, .T. ) ;
#11390 = CARTESIAN_POINT ( 'NONE',  ( 82.40000000000000568, -33.03750000000000142, -102.9999999999999858 ) ) ;
#11391 = CARTESIAN_POINT ( 'NONE',  ( 84.12112955302457351, -35.00000000000000000, -97.53419980903892395 ) ) ;
#11392 =( BOUNDED_CURVE ( )  B_SPLINE_CURVE ( 2, ( #17587, #8492, #3808, #6760, #898, #11622, #1178, #14447, #11240 ),
 .UNSPECIFIED., .F., .F. ) 
 B_SPLINE_CURVE_WITH_KNOTS ( ( 3, 2, 2, 2, 3 ),
 ( 0.3958333333333333703, 0.4027777777777777901, 0.4166666666666666852, 0.4305555555555555802, 0.4375000000000001110 ),
 .UNSPECIFIED. ) 
 CURVE ( )  GEOMETRIC_REPRESENTATION_ITEM ( )  RATIONAL_B_SPLINE_CURVE ( ( 0.9330127018922194093, 0.9330127018922196314, 1.000000000000000000, 0.8660254037844387076, 1.000000000000000000, 0.8660254037844387076, 1.000000000000000000, 0.9330127018922182991, 0.9330127018922194093 ) ) 
 REPRESENTATION_ITEM ( '' )  );
#11393 = CARTESIAN_POINT ( 'NONE',  ( -79.39999999999999147, -31.12106250001229313, 99.99999999999998579 ) ) ;
#11394 = EDGE_CURVE ( 'NONE', #13993, #5913, #13297, .T. ) ;
#11395 = CARTESIAN_POINT ( 'NONE',  ( 4.033901012035826739, 3.740908793663638487, -0.5205559028932524868 ) ) ;
#11396 = CARTESIAN_POINT ( 'NONE',  ( 83.20384757729335945, -34.08615380933863293, -96.99999999999998579 ) ) ;
#11397 = CARTESIAN_POINT ( 'NONE',  ( -83.20384757729338787, -34.53615380933862866, 97.00000000000000000 ) ) ;
#11398 = CARTESIAN_POINT ( 'NONE',  ( -83.20384757729335945, -32.73615380933863150, 96.99999999999998579 ) ) ;
#11399 = DIRECTION ( 'NONE',  ( 1.000000000000000000, 0.000000000000000000, 0.000000000000000000 ) ) ;
#11400 =( BOUNDED_CURVE ( )  B_SPLINE_CURVE ( 2, ( #3599, #9561, #12877, #17285, #19035, #14429, #9955, #11319, #5659 ),
 .UNSPECIFIED., .F., .F. ) 
 B_SPLINE_CURVE_WITH_KNOTS ( ( 3, 2, 2, 2, 3 ),
 ( 0.5625000000000000000, 0.5694444444444444198, 0.5833333333333333703, 0.5972222222222222099, 0.6041666666666666297 ),
 .UNSPECIFIED. ) 
 CURVE ( )  GEOMETRIC_REPRESENTATION_ITEM ( )  RATIONAL_B_SPLINE_CURVE ( ( 0.9330127018922194093, 0.9330127018922194093, 1.000000000000000000, 0.8660254037844387076, 1.000000000000000000, 0.8660254037844387076, 1.000000000000000000, 0.9330127018922198534, 0.9330127018922192983 ) ) 
 REPRESENTATION_ITEM ( '' )  );
#11401 = CARTESIAN_POINT ( 'NONE',  ( -6.468631247035699870E-16, -3.375361811986504534, 1.153701847711635198 ) ) ;
#11402 = CARTESIAN_POINT ( 'NONE',  ( 229.5999999999999375, -34.89374999877096428, -50.00000000000011369 ) ) ;
#11403 = CARTESIAN_POINT ( 'NONE',  ( 82.39999999999999147, -34.86562499938548854, -96.81714838363319586 ) ) ;
#11404 = CARTESIAN_POINT ( 'NONE',  ( 231.0999999999999375, -33.97500000000000142, 102.5980762113533018 ) ) ;
#11405 = PRESENTATION_LAYER_ASSIGNMENT (  '', '', ( #12637 ) ) ;
#11406 = VERTEX_POINT ( 'NONE', #1214 ) ;
#11407 = CARTESIAN_POINT ( 'NONE',  ( 85.40000000000000568, -34.03124999877096712, 101.7320508075688679 ) ) ;
#11408 = CONTEXT_DEPENDENT_SHAPE_REPRESENTATION ( #4215, #953 ) ;
#11409 = CARTESIAN_POINT ( 'NONE',  ( 235.3564303562499447, -34.97812499938547859, 99.99999999999998579 ) ) ;
#11410 = CARTESIAN_POINT ( 'NONE',  ( 229.8435696437499871, -32.99062499938548143, -51.59142580818350865 ) ) ;
#11411 = LINE ( 'NONE', #16098, #16162 ) ;
#11412 = B_SPLINE_CURVE_WITH_KNOTS ( 'NONE', 3,
 ( #17701, #17319, #19170, #4317, #18981, #10278, #10175, #7242, #16240, #2847, #8803, #5411, #11354, #4122, #9894, #2464, #8419, #14373 ),
 .UNSPECIFIED., .F., .F.,
 ( 4, 2, 2, 2, 2, 2, 2, 2, 4 ),
 ( 0.000000000000000000, 0.0007089252359835979036, 0.001417850471967195807, 0.002126775707950793494, 0.002835700943934391614, 0.003544626179917989735, 0.004253551415901586988, 0.004962476651885185108, 0.005671401887868783229 ),
 .UNSPECIFIED. ) ;
#11413 = DIRECTION ( 'NONE',  ( 1.000000000000000000, 0.000000000000000000, -0.000000000000000000 ) ) ;
#11414 = ORIENTED_EDGE ( 'NONE', *, *, #3381, .T. ) ;
#11415 = CARTESIAN_POINT ( 'NONE',  ( -79.64356964375001269, -32.20312499938548001, -98.40857419181659793 ) ) ;
#11416 = FACE_OUTER_BOUND ( 'NONE', #5673, .T. ) ;
#11417 = ORIENTED_EDGE ( 'NONE', *, *, #18544, .T. ) ;
#11418 = CARTESIAN_POINT ( 'NONE',  ( 82.39999999999999147, -33.06562499938548427, 103.1828516163667899 ) ) ;
#11419 = CARTESIAN_POINT ( 'NONE',  ( -81.02178482187500208, -31.30312499938548498, -102.3871387122750889 ) ) ;
#11420 = AXIS2_PLACEMENT_3D ( 'NONE', #15303, #472, #8077 ) ;
#11421 = CARTESIAN_POINT ( 'NONE',  ( 82.39999999999999147, -34.16250000000000142, 103.4641016151377499 ) ) ;
#11422 = CARTESIAN_POINT ( 'NONE',  ( 80.90000000000000568, -34.59374999877096712, -97.40192378864668399 ) ) ;
#11423 = CARTESIAN_POINT ( 'NONE',  ( -79.39999999999999147, -33.80624999877097281, 101.7320508075688537 ) ) ;
#11424 = CARTESIAN_POINT ( 'NONE',  ( -83.77821517812500929, -31.52812499938548996, 102.3871387122750889 ) ) ;
#11425 = CARTESIAN_POINT ( 'NONE',  ( -85.15643035625001289, -33.29062499938547859, -99.99999999999998579 ) ) ;
#11426 =( BOUNDED_CURVE ( )  B_SPLINE_CURVE ( 2, ( #10790, #15386, #7956, #1999, #15681, #455, #14201, #6404, #12357, #14012, #13910, #548, #648, #6506, #12451, #6597, #5038, #9624, #10980, #9520, #12545, #18516, #17047, #3659, #8534, #13031, #5337, #10106, #18809, #14483, #15775, #17531, #2666, #12747, #8345, #15876, #9813, #4146, #1115, #14300, #15965, #16062, #13122, #2572, #14581, #7072, #19002, #5622, #2383, #10009, #18714, #18903, #936, #8627, #11568, #1216, #7172, #6800, #11274, #6891, #17243, #8438, #14390, #3847, #12841, #4050, #2480, #5434, #11371, #1029, #17338, #5524, #3948, #11472, #9913, #17439, #6981, #12933, #14176, #2067, #18396, #6673, #12615 ),
 .UNSPECIFIED., .F., .F. ) 
 B_SPLINE_CURVE_WITH_KNOTS ( ( 3, 2, 2, 2, 2, 2, 2, 2, 2, 2, 2, 2, 2, 2, 2, 2, 2, 2, 2, 2, 2, 2, 2, 2, 2, 2, 2, 2, 2, 2, 2, 2, 2, 2, 2, 2, 2, 2, 2, 2, 2, 3 ),
 ( 0.3495698921800971526, 0.3600184345287979482, 0.3750192026341645501, 0.3900199707395311521, 0.4050207388448977541, 0.4200215069502643561, 0.4350222750556309581, 0.4500230431609975046, 0.4650238112663641066, 0.4800245793717306531, 0.4950253474770972550, 0.5100261155824639125, 0.5250268836878304590, 0.5400276517931970055, 0.5550284198985635520, 0.5700291880039302095, 0.5850299561092967560, 0.6000307242146634135, 0.6150314923200299599, 0.6300322604253966174, 0.6450330285307630529, 0.6600337966361298214, 0.6750345647414963679, 0.6900353328468629144, 0.7050361009522294609, 0.7200368690575960073, 0.7350376371629626648, 0.7500384052683292113, 0.7650391733736958688, 0.7800399414790624153, 0.7950407095844290728, 0.8100414776897955083, 0.8250422457951621658, 0.8400430139005288233, 0.8550437820058952587, 0.8700445501112620272, 0.8850453182166284627, 0.9000460863219952312, 0.9150468544273616667, 0.9300476225327284352, 0.9450483906380948707, 0.9496006163947589007 ),
 .UNSPECIFIED. ) 
 CURVE ( )  GEOMETRIC_REPRESENTATION_ITEM ( )  RATIONAL_B_SPLINE_CURVE ( ( 0.9433623850486676510, 0.9066821623815660702, 1.000000000000000000, 0.8660254037844387076, 1.000000000000000000, 0.8660254037844387076, 1.000000000000000000, 0.8660254037844387076, 1.000000000000000000, 0.8660254037844387076, 1.000000000000000000, 0.8660254037844387076, 1.000000000000000000, 0.8660254037844387076, 1.000000000000000000, 0.8660254037844387076, 1.000000000000000000, 0.8660254037844387076, 1.000000000000000000, 0.8660254037844387076, 1.000000000000000000, 0.8660254037844387076, 1.000000000000000000, 0.8660254037844387076, 1.000000000000000000, 0.8660254037844387076, 1.000000000000000000, 0.8660254037844387076, 1.000000000000000000, 0.8660254037844387076, 1.000000000000000000, 0.8660254037844387076, 1.000000000000000000, 0.8660254037844387076, 1.000000000000000000, 0.8660254037844387076, 1.000000000000000000, 0.8660254037844387076, 1.000000000000000000, 0.8660254037844387076, 1.000000000000000000, 0.8660254037844387076, 1.000000000000000000, 0.8660254037844387076, 1.000000000000000000, 0.8660254037844387076, 1.000000000000000000, 0.8660254037844387076, 1.000000000000000000, 0.8660254037844387076, 1.000000000000000000, 0.8660254037844387076, 1.000000000000000000, 0.8660254037844387076, 1.000000000000000000, 0.8660254037844387076, 1.000000000000000000, 0.8660254037844387076, 1.000000000000000000, 0.8660254037844387076, 1.000000000000000000, 0.8660254037844387076, 1.000000000000000000, 0.8660254037844387076, 1.000000000000000000, 0.8660254037844387076, 1.000000000000000000, 0.8660254037844387076, 1.000000000000000000, 0.8660254037844387076, 1.000000000000000000, 0.8660254037844387076, 1.000000000000000000, 0.8660254037844387076, 1.000000000000000000, 0.8660254037844387076, 1.000000000000000000, 0.8660254037844387076, 1.000000000000000000, 0.8660254037844387076, 1.000000000000000000, 0.9593432414028885136, 0.9433623850486800855 ) ) 
 REPRESENTATION_ITEM ( '' )  );
#11427 = CARTESIAN_POINT ( 'NONE',  ( 230.8788704469753839, -35.00000000000000000, 97.53419980903893816 ) ) ;
#11428 = CARTESIAN_POINT ( 'NONE',  ( 85.40000000000000568, -31.70624999877096784, -101.7320508075688679 ) ) ;
#11429 = CARTESIAN_POINT ( 'NONE',  ( 229.5999999999999375, -30.89999999999999858, 99.99999999999998579 ) ) ;
#11430 = AXIS2_PLACEMENT_3D ( 'NONE', #1840, #6056, #10821 ) ;
#11431 = VERTEX_POINT ( 'NONE', #18901 ) ;
#11432 = CARTESIAN_POINT ( 'NONE',  ( 85.15643035625001289, -33.74062499938548854, -99.99999999999998579 ) ) ;
#11433 = ADVANCED_FACE ( 'NONE', ( #7070 ), #19000, .F. ) ;
#11434 = CARTESIAN_POINT ( 'NONE',  ( 229.5999999999999375, -32.15624999877096002, 101.7320508075688679 ) ) ;
#11435 = CARTESIAN_POINT ( 'NONE',  ( 232.5999999999999375, -30.50624999877096144, -53.46410161513786363 ) ) ;
#11436 = AXIS2_PLACEMENT_3D ( 'NONE', #5829, #7191, #2594 ) ;
#11437 = CARTESIAN_POINT ( 'NONE',  ( -81.02178482187500208, -32.24062499938548854, 102.3871387122750889 ) ) ;
#11438 = ORIENTED_EDGE ( 'NONE', *, *, #18097, .F. ) ;
#11439 = EDGE_LOOP ( 'NONE', ( #18486, #16510, #897, #919 ) ) ;
#11440 = CARTESIAN_POINT ( 'NONE',  ( -83.20384757729335945, -33.90134618820329848, -96.99999999999998579 ) ) ;
#11441 = CARTESIAN_POINT ( 'NONE',  ( 235.5999999999999375, -33.76874999877096428, -50.00000000000011369 ) ) ;
#11442 = ORIENTED_EDGE ( 'NONE', *, *, #4465, .F. ) ;
#11443 =( NAMED_UNIT ( * ) SI_UNIT ( $, .STERADIAN. ) SOLID_ANGLE_UNIT ( ) );
#11444 = CARTESIAN_POINT ( 'NONE',  ( 83.90000000000000568, -32.17500000000000426, -102.5980762113533018 ) ) ;
#11445 = CYLINDRICAL_SURFACE ( 'NONE', #5518, 3.000000000000002665 ) ;
#11446 = B_SPLINE_CURVE_WITH_KNOTS ( 'NONE', 3,
 ( #15989, #8554, #14506, #1140, #19021, #11873, #11970, #4752, #263, #1531, #14801, #3266, #12068, #1428, #8937, #5927 ),
 .UNSPECIFIED., .F., .F.,
 ( 4, 2, 2, 2, 2, 2, 2, 4 ),
 ( 0.000000000000000000, 0.0005391024520904015354, 0.001078204904180803071, 0.002156409808361606142, 0.002695512260452029903, 0.003234614712542453665, 0.003773717164632876993, 0.004312819616723300754 ),
 .UNSPECIFIED. ) ;
#11447 = CARTESIAN_POINT ( 'NONE',  ( -83.77821517812500929, -32.42812499938548854, 102.3871387122750889 ) ) ;
#11448 = CARTESIAN_POINT ( 'NONE',  ( -82.39999999999999147, -33.26250000000000284, 96.53589838486223584 ) ) ;
#11449 = CARTESIAN_POINT ( 'NONE',  ( 4.211140560182196957, 2.431303136016536470, -3.745885042887433514 ) ) ;
#11450 = CARTESIAN_POINT ( 'NONE',  ( 111.5000000000000142, 12.69999999999998508, 50.00000000000001421 ) ) ;
#11451 = CARTESIAN_POINT ( 'NONE',  ( 79.64356964374998427, -32.12812499938548427, 101.5914258081833879 ) ) ;
#11452 = LINE ( 'NONE', #11733, #3379 ) ;
#11453 = CARTESIAN_POINT ( 'NONE',  ( -85.15643035624999868, -35.11426555956768425, 98.99674139749697588 ) ) ;
#11454 = FACE_OUTER_BOUND ( 'NONE', #10177, .T. ) ;
#11455 = ORIENTED_EDGE ( 'NONE', *, *, #19036, .F. ) ;
#11456 = VECTOR ( 'NONE', #1719, 1000.000000000000000 ) ;
#11457 = CARTESIAN_POINT ( 'NONE',  ( 234.0999999999999375, -34.35000000000000142, -47.40192378864679768 ) ) ;
#11458 = CARTESIAN_POINT ( 'NONE',  ( -81.59615242270662350, -33.22634618820330132, 96.99999999999998579 ) ) ;
#11459 = DIRECTION ( 'NONE',  ( 0.000000000000000000, 0.000000000000000000, -1.000000000000000000 ) ) ;
#11460 = CARTESIAN_POINT ( 'NONE',  ( -79.64356964375001269, -34.11562499938548854, 101.5914258081833879 ) ) ;
#11461 = CARTESIAN_POINT ( 'NONE',  ( 231.2217848218749339, -30.51562499938548001, -47.61286128772501769 ) ) ;
#11462 = AXIS2_PLACEMENT_3D ( 'NONE', #13577, #3223, #9181 ) ;
#11463 =( BOUNDED_CURVE ( )  B_SPLINE_CURVE ( 2, ( #9654, #18161, #2219, #4784, #3588, #6435, #4876, #6626, #10726 ),
 .UNSPECIFIED., .F., .F. ) 
 B_SPLINE_CURVE_WITH_KNOTS ( ( 3, 2, 2, 2, 3 ),
 ( 0.8541666666666665186, 0.8611111111111111605, 0.8750000000000000000, 0.8888888888888888395, 0.8958333333333333703 ),
 .UNSPECIFIED. ) 
 CURVE ( )  GEOMETRIC_REPRESENTATION_ITEM ( )  RATIONAL_B_SPLINE_CURVE ( ( 0.9330127018922194093, 0.9330127018922177440, 1.000000000000000000, 0.8660254037844387076, 1.000000000000000000, 0.8660254037844387076, 1.000000000000000000, 0.9330127018922187432, 0.9330127018922192983 ) ) 
 REPRESENTATION_ITEM ( '' )  );
#11464 = ORIENTED_EDGE ( 'NONE', *, *, #17948, .T. ) ;
#11465 = CARTESIAN_POINT ( 'NONE',  ( -79.64356964374999848, -34.41562499938548569, 99.99999999999998579 ) ) ;
#11466 = CARTESIAN_POINT ( 'NONE',  ( 82.40000000000001990, -34.55624999877097281, 103.0000000000000000 ) ) ;
#11467 = CARTESIAN_POINT ( 'NONE',  ( 81.02178482187500208, -34.94062499938548427, 97.61286128772489690 ) ) ;
#11468 = EDGE_CURVE ( 'NONE', #6376, #6906, #4542, .T. ) ;
#11469 = DIRECTION ( 'NONE',  ( -0.000000000000000000, -0.000000000000000000, -1.000000000000000000 ) ) ;
#11470 = CARTESIAN_POINT ( 'NONE',  ( -4.000000000000000000, 2.309401076758498483, -3.433295621305379353 ) ) ;
#11471 = CARTESIAN_POINT ( 'NONE',  ( -79.64356964374999848, -34.97812499938548569, 99.99999999999998579 ) ) ;
#11472 = CARTESIAN_POINT ( 'NONE',  ( -85.15643035625001289, -34.71562499938548285, -98.40857419181659793 ) ) ;
#11473 = CARTESIAN_POINT ( 'NONE',  ( 85.15643035624999868, -32.35312499938549280, 98.40857419181659793 ) ) ;
#11474 = CARTESIAN_POINT ( 'NONE',  ( 81.02178482187500208, -34.00312499938548427, -97.61286128772489690 ) ) ;
#11475 = CARTESIAN_POINT ( 'NONE',  ( 231.2217848218749339, -34.11562499938548143, -47.61286128772501769 ) ) ;
#11476 = CARTESIAN_POINT ( 'NONE',  ( -79.64356964374999848, -32.16562499938548569, 99.99999999999998579 ) ) ;
#11477 = CARTESIAN_POINT ( 'NONE',  ( 85.15643035624999868, -31.90312499938548285, -101.5914258081833879 ) ) ;
#11478 = ORIENTED_EDGE ( 'NONE', *, *, #8247, .T. ) ;
#11479 = FACE_OUTER_BOUND ( 'NONE', #5342, .T. ) ;
#11480 = CONICAL_SURFACE ( 'NONE', #13970, 2.500000000000000888, 0.9599310885968785900 ) ;
#11481 = PLANE ( 'NONE',  #6185 ) ;
#11482 = CARTESIAN_POINT ( 'NONE',  ( -85.40000000000000568, -34.46249999999999858, 101.7320508075688679 ) ) ;
#11483 = CARTESIAN_POINT ( 'NONE',  ( -82.39999999999999147, -33.85312499938547859, 96.81714838363319586 ) ) ;
#11484 = CARTESIAN_POINT ( 'NONE',  ( -83.77821517812500929, -30.66562499938548569, 97.61286128772489690 ) ) ;
#11485 = VERTEX_POINT ( 'NONE', #18806 ) ;
#11486 = DIRECTION ( 'NONE',  ( 5.139921410301648824E-16, 1.000000000000000000, 0.000000000000000000 ) ) ;
#11487 = VECTOR ( 'NONE', #8354, 1000.000000000000000 ) ;
#11488 = VECTOR ( 'NONE', #14554, 1000.000000000000000 ) ;
#11489 = DIRECTION ( 'NONE',  ( 1.387778780781445676E-15, 1.000000000000000000, 0.000000000000000000 ) ) ;
#11490 = CARTESIAN_POINT ( 'NONE',  ( 82.41196654184807358, -34.99999999999999289, -97.00083539721711645 ) ) ;
#11491 = CARTESIAN_POINT ( 'NONE',  ( -83.90000000000000568, -30.37106250001229313, 102.5980762113533018 ) ) ;
#11492 = CARTESIAN_POINT ( 'NONE',  ( -82.40000000000000568, -34.61250000000001137, 97.00000000000000000 ) ) ;
#11493 = AXIS2_PLACEMENT_3D ( 'NONE', #13133, #5635, #4444 ) ;
#11494 = CARTESIAN_POINT ( 'NONE',  ( -85.40000000000000568, -34.89374999877097139, 99.99999999999998579 ) ) ;
#11495 = CARTESIAN_POINT ( 'NONE',  ( -79.39999999999999147, -33.31874999877096855, -99.99999999999998579 ) ) ;
#11496 = CARTESIAN_POINT ( 'NONE',  ( -85.40000000000000568, -33.63750000000000284, 98.26794919243111792 ) ) ;
#11497 = CARTESIAN_POINT ( 'NONE',  ( -85.40000000000000568, -33.13124999877096855, -101.7320508075688821 ) ) ;
#11498 = DIRECTION ( 'NONE',  ( -0.000000000000000000, -1.000000000000000000, -0.000000000000000000 ) ) ;
#11499 = CARTESIAN_POINT ( 'NONE',  ( 99.99999999999994316, -21.80000000000003268, -139.9999999999999716 ) ) ;
#11500 = CARTESIAN_POINT ( 'NONE',  ( 79.64356964375001269, -34.04062499938549280, -98.40857419181659793 ) ) ;
#11501 = AXIS2_PLACEMENT_3D ( 'NONE', #15946, #2748, #5780 ) ;
#11502 = CARTESIAN_POINT ( 'NONE',  ( -83.90000000000000568, -33.01874999877097139, 102.5980762113533018 ) ) ;
#11503 = EDGE_CURVE ( 'NONE', #3766, #9169, #15773, .T. ) ;
#11504 = EDGE_LOOP ( 'NONE', ( #878, #18818, #14788, #14111, #18084, #16675, #3048, #10827, #2952, #7707, #16560, #14735, #3038, #2035, #5846, #9195, #14427 ) ) ;
#11505 = CARTESIAN_POINT ( 'NONE',  ( 82.39999999999999147, -33.88124999877096855, 96.53589838486223584 ) ) ;
#11506 = CONTEXT_DEPENDENT_SHAPE_REPRESENTATION ( #6591, #14028 ) ;
#11507 = CARTESIAN_POINT ( 'NONE',  ( 229.8435696437499303, -34.30312499938548143, 99.99999999999998579 ) ) ;
#11508 = CARTESIAN_POINT ( 'NONE',  ( 235.3564303562499447, -32.24062499938548143, -51.59142580818350865 ) ) ;
#11509 = DIRECTION ( 'NONE',  ( -1.000000000000000000, -0.000000000000000000, -0.000000000000000000 ) ) ;
#11510 = CARTESIAN_POINT ( 'NONE',  ( 0.000000000000000000, 0.000000000000000000, -4.974599999999998801 ) ) ;
#11511 = ORIENTED_EDGE ( 'NONE', *, *, #13311, .T. ) ;
#11512 = CARTESIAN_POINT ( 'NONE',  ( -82.39999999999999147, -33.17812499938548854, -96.81714838363319586 ) ) ;
#11513 = LINE ( 'NONE', #15816, #10056 ) ;
#11514 = EDGE_CURVE ( 'NONE', #5649, #8302, #16060, .T. ) ;
#11515 = VERTEX_POINT ( 'NONE', #10007 ) ;
#11516 = CARTESIAN_POINT ( 'NONE',  ( -83.90000000000000568, -32.26874999877097139, 97.40192378864668399 ) ) ;
#11517 = CARTESIAN_POINT ( 'NONE',  ( -83.77821517812500929, -30.32812499938548711, -102.3871387122750889 ) ) ;
#11518 =( BOUNDED_CURVE ( )  B_SPLINE_CURVE ( 2, ( #15309, #1922, #6621, #12570, #7885, #13836, #478, #12475, #6429 ),
 .UNSPECIFIED., .F., .F. ) 
 B_SPLINE_CURVE_WITH_KNOTS ( ( 3, 2, 2, 2, 3 ),
 ( 0.8125000000000000000, 0.8194444444444444198, 0.8333333333333333703, 0.8472222222222222099, 0.8541666666666665186 ),
 .UNSPECIFIED. ) 
 CURVE ( )  GEOMETRIC_REPRESENTATION_ITEM ( )  RATIONAL_B_SPLINE_CURVE ( ( 0.9330127018922194093, 0.9330127018922194093, 1.000000000000000000, 0.8660254037844387076, 1.000000000000000000, 0.8660254037844387076, 1.000000000000000000, 0.9330127018922209636, 0.9330127018922194093 ) ) 
 REPRESENTATION_ITEM ( '' )  );
#11519 = CARTESIAN_POINT ( 'NONE',  ( 85.39999999999999147, -34.97364041986484295, 101.0919042218176287 ) ) ;
#11520 = CARTESIAN_POINT ( 'NONE',  ( -81.70916641599835373, -34.99999999999998579, 97.11314983874014217 ) ) ;
#11521 = CARTESIAN_POINT ( 'NONE',  ( -80.90000000000000568, -34.14374999877097139, 97.40192378864668399 ) ) ;
#11522 = CARTESIAN_POINT ( 'NONE',  ( -82.39999999999999147, -30.59062499938548640, 103.1828516163667899 ) ) ;
#11523 = CARTESIAN_POINT ( 'NONE',  ( -79.64356964374998427, -33.10312499938548569, -98.40857419181659793 ) ) ;
#11524 = CARTESIAN_POINT ( 'NONE',  ( 105.5000000000000142, 12.69999999999998508, 50.00000000000001421 ) ) ;
#11525 = EDGE_CURVE ( 'NONE', #13878, #10068, #5484, .T. ) ;
#11526 = CARTESIAN_POINT ( 'NONE',  ( 83.90000000000000568, -32.56874999877096855, -102.5980762113533018 ) ) ;
#11527 = CARTESIAN_POINT ( 'NONE',  ( 235.5999999999999943, -31.08749999999999503, 98.26794919243110371 ) ) ;
#11528 = EDGE_CURVE ( 'NONE', #7316, #13275, #2684, .T. ) ;
#11529 = VERTEX_POINT ( 'NONE', #4240 ) ;
#11530 = CARTESIAN_POINT ( 'NONE',  ( 235.5999999999999943, -33.28124999877096002, 98.26794919243110371 ) ) ;
#11531 = CARTESIAN_POINT ( 'NONE',  ( 229.5999999999999375, -30.39374999877096428, -50.00000000000011369 ) ) ;
#11532 = EDGE_CURVE ( 'NONE', #3690, #6638, #2570, .T. ) ;
#11533 = CARTESIAN_POINT ( 'NONE',  ( -85.40000000000000568, -35.30624999877096570, 101.7320508075688821 ) ) ;
#11534 = CARTESIAN_POINT ( 'NONE',  ( -81.02178482187500208, -31.79062499938548925, 102.3871387122750889 ) ) ;
#11535 = ORIENTED_EDGE ( 'NONE', *, *, #14731, .F. ) ;
#11536 = ORIENTED_EDGE ( 'NONE', *, *, #9640, .F. ) ;
#11537 = CARTESIAN_POINT ( 'NONE',  ( -4.198928548860774157, 0.8158838809860065044, -3.526471437616918170 ) ) ;
#11538 = CARTESIAN_POINT ( 'NONE',  ( 4.175813232069146785, 2.061359961916366057, -3.570380186727397653 ) ) ;
#11539 = VERTEX_POINT ( 'NONE', #12724 ) ;
#11540 = SURFACE_STYLE_USAGE ( .BOTH. , #3917 ) ;
#11541 = CARTESIAN_POINT ( 'NONE',  ( 83.90000000000000568, -31.72500000000000142, -102.5980762113533018 ) ) ;
#11542 = CARTESIAN_POINT ( 'NONE',  ( 0.2182387239031248483, 1.693823289467350390, 3.500000000000000000 ) ) ;
#11543 = CARTESIAN_POINT ( 'NONE',  ( -83.77821517812500929, -30.77812499938548640, 97.61286128772489690 ) ) ;
#11544 = CARTESIAN_POINT ( 'NONE',  ( -80.90000000000000568, -31.05000000000000071, 97.40192378864668399 ) ) ;
#11545 = EDGE_CURVE ( 'NONE', #1971, #14449, #6580, .T. ) ;
#11546 = DIRECTION ( 'NONE',  ( -0.000000000000000000, -1.000000000000000000, -0.000000000000000000 ) ) ;
#11547 = CARTESIAN_POINT ( 'NONE',  ( -82.40000000000001990, -32.75624999877096855, 97.00000000000000000 ) ) ;
#11548 = DIRECTION ( 'NONE',  ( -0.000000000000000000, -1.000000000000000000, -0.000000000000000000 ) ) ;
#11549 = CARTESIAN_POINT ( 'NONE',  ( 5.599999999999999645, 0.000000000000000000, 0.000000000000000000 ) ) ;
#11550 = DIRECTION ( 'NONE',  ( 0.000000000000000000, 0.000000000000000000, -1.000000000000000000 ) ) ;
#11551 = EDGE_LOOP ( 'NONE', ( #6459, #16410, #397, #7736 ) ) ;
#11552 = CARTESIAN_POINT ( 'NONE',  ( -83.77821517812500929, -31.41562499938548569, -97.61286128772489690 ) ) ;
#11553 = CARTESIAN_POINT ( 'NONE',  ( 235.3594282536526237, -35.00000000000000000, 100.3964642588227605 ) ) ;
#11554 = CARTESIAN_POINT ( 'NONE',  ( -85.15643035625001289, -30.25312499938548783, 99.99999999999998579 ) ) ;
#11555 = DIRECTION ( 'NONE',  ( 2.312964634635736745E-15, 1.000000000000000000, 0.000000000000000000 ) ) ;
#11556 = CARTESIAN_POINT ( 'NONE',  ( -83.77821517812500929, -33.32812499938548711, 102.3871387122750889 ) ) ;
#11557 = CARTESIAN_POINT ( 'NONE',  ( 81.59615242270662350, -32.38259618943233420, 102.9999999999999716 ) ) ;
#11558 = EDGE_CURVE ( 'NONE', #16799, #4468, #3316, .T. ) ;
#11559 = CARTESIAN_POINT ( 'NONE',  ( 231.2217848218749339, -30.96562499938547930, -47.61286128772501769 ) ) ;
#11560 = VERTEX_POINT ( 'NONE', #11547 ) ;
#11561 = CARTESIAN_POINT ( 'NONE',  ( -79.64356964374999848, -33.06562499938548427, 99.99999999999998579 ) ) ;
#11562 = CARTESIAN_POINT ( 'NONE',  ( -82.40000000000000568, -33.93750000000000711, -97.00000000000000000 ) ) ;
#11563 = CARTESIAN_POINT ( 'NONE',  ( 79.39999999999999147, -30.18750000000000355, 101.7320508075688821 ) ) ;
#11564 = CARTESIAN_POINT ( 'NONE',  ( -82.40000000000000568, -34.38749999999999574, 102.9999999999999858 ) ) ;
#11565 = CARTESIAN_POINT ( 'NONE',  ( 233.9782151781249411, -30.74062499938547788, 97.61286128772489690 ) ) ;
#11566 = CARTESIAN_POINT ( 'NONE',  ( 99.99999999999997158, -5.200000000000008171, 150.0000000000000000 ) ) ;
#11567 = CARTESIAN_POINT ( 'NONE',  ( -79.64356964374998427, -34.11562499938548854, 101.5914258081833879 ) ) ;
#11568 = CARTESIAN_POINT ( 'NONE',  ( -81.02178482187500208, -34.00312499938548427, -102.3871387122750889 ) ) ;
#11569 = CARTESIAN_POINT ( 'NONE',  ( 81.02178482187500208, -33.44062499938548427, 102.3871387122750889 ) ) ;
#11570 = CARTESIAN_POINT ( 'NONE',  ( 85.15643035624999868, -34.79062499938548569, -98.40857419181659793 ) ) ;
#11571 = CARTESIAN_POINT ( 'NONE',  ( 231.1166048115126443, -35.16733441503057378, -52.52040863755893696 ) ) ;
#11572 = CARTESIAN_POINT ( 'NONE',  ( -82.39999999999999147, -34.07812499938548711, 103.1828516163667899 ) ) ;
#11573 = CARTESIAN_POINT ( 'NONE',  ( 85.15643035624999868, -31.07812499938548356, -98.40857419181659793 ) ) ;
#11574 = ORIENTED_EDGE ( 'NONE', *, *, #323, .F. ) ;
#11575 = CARTESIAN_POINT ( 'NONE',  ( 83.77821517812500929, -34.67812499938548854, 97.61286128772489690 ) ) ;
#11576 = CARTESIAN_POINT ( 'NONE',  ( 2.725741868436127202, -3.045094352033990148, -3.220599429844051453 ) ) ;
#11577 = CARTESIAN_POINT ( 'NONE',  ( -80.90000000000000568, -32.85000000000000142, 97.40192378864668399 ) ) ;
#11578 = CARTESIAN_POINT ( 'NONE',  ( -81.02178482187500208, -33.44062499938548427, 97.61286128772489690 ) ) ;
#11579 = CARTESIAN_POINT ( 'NONE',  ( -79.64356964375001269, -31.75312499938548427, 101.5914258081833879 ) ) ;
#11580 = ORIENTED_EDGE ( 'NONE', *, *, #10348, .T. ) ;
#11581 = CARTESIAN_POINT ( 'NONE',  ( -85.40000000000000568, -30.45000000000000284, 99.99999999999998579 ) ) ;
#11582 = CARTESIAN_POINT ( 'NONE',  ( 233.9782151781249411, -32.24062499938548143, 102.3871387122750889 ) ) ;
#11583 = CARTESIAN_POINT ( 'NONE',  ( 80.03686793005721256, -35.00000000000000711, -98.35371953419867452 ) ) ;
#11584 = CARTESIAN_POINT ( 'NONE',  ( -79.39999999999999147, -30.25856250001228887, 101.7320508075688537 ) ) ;
#11585 = CARTESIAN_POINT ( 'NONE',  ( -79.39999999999999147, -34.68750000000000000, 98.26794919243110371 ) ) ;
#11586 = CARTESIAN_POINT ( 'NONE',  ( 83.90000000000000568, -33.91874999877096997, -102.5980762113533018 ) ) ;
#11587 = CARTESIAN_POINT ( 'NONE',  ( -81.02178482187500208, -30.29062499938548569, 97.61286128772489690 ) ) ;
#11588 = FACE_OUTER_BOUND ( 'NONE', #17985, .T. ) ;
#11589 = CARTESIAN_POINT ( 'NONE',  ( 81.02178482187500208, -33.25312499938548427, 97.61286128772489690 ) ) ;
#11590 = PLANE ( 'NONE',  #13007 ) ;
#11591 = CARTESIAN_POINT ( 'NONE',  ( -82.40000000000001990, -32.75624999877096855, -103.0000000000000000 ) ) ;
#11592 = CARTESIAN_POINT ( 'NONE',  ( 81.02178482187500208, -34.00312499938548427, -97.61286128772489690 ) ) ;
#11593 = DIRECTION ( 'NONE',  ( -1.387778780781445676E-15, -1.000000000000000000, 0.000000000000000000 ) ) ;
#11594 = ORIENTED_EDGE ( 'NONE', *, *, #12830, .F. ) ;
#11595 = CARTESIAN_POINT ( 'NONE',  ( 79.39999999999999147, -33.35624999877097707, 98.26794919243113213 ) ) ;
#11596 = CARTESIAN_POINT ( 'NONE',  ( 229.8435696437499871, -34.71562499938548285, 101.5914258081833879 ) ) ;
#11597 = CARTESIAN_POINT ( 'NONE',  ( 83.90000000000000568, -32.71874999877096712, 102.5980762113533018 ) ) ;
#11598 = DIRECTION ( 'NONE',  ( 0.000000000000000000, 0.000000000000000000, 1.000000000000000000 ) ) ;
#11599 = DIRECTION ( 'NONE',  ( -1.000000000000000000, 0.000000000000000000, 0.000000000000000000 ) ) ;
#11600 = VERTEX_POINT ( 'NONE', #17218 ) ;
#11601 = CARTESIAN_POINT ( 'NONE',  ( -79.64356964375001269, -34.45312499938548711, -98.40857419181659793 ) ) ;
#11602 = DIRECTION ( 'NONE',  ( 0.000000000000000000, -0.000000000000000000, -1.000000000000000000 ) ) ;
#11603 = EDGE_LOOP ( 'NONE', ( #7963, #5245, #6444, #2156 ) ) ;
#11604 = DIRECTION ( 'NONE',  ( 0.000000000000000000, 0.000000000000000000, -1.000000000000000000 ) ) ;
#11605 = CARTESIAN_POINT ( 'NONE',  ( -83.77821517812500929, -30.77812499938548640, -102.3871387122750889 ) ) ;
#11606 = CARTESIAN_POINT ( 'NONE',  ( -85.40000000000000568, -31.29374999877096997, -99.99999999999998579 ) ) ;
#11607 = CARTESIAN_POINT ( 'NONE',  ( 79.39999999999999147, -34.66874999877096997, -99.99999999999998579 ) ) ;
#11608 = CARTESIAN_POINT ( 'NONE',  ( -79.39999999999999147, -33.73124999877096997, 98.26794919243110371 ) ) ;
#11609 = CARTESIAN_POINT ( 'NONE',  ( -81.02178482187500208, -32.20312499938548711, 97.61286128772489690 ) ) ;
#11610 = CARTESIAN_POINT ( 'NONE',  ( -81.59615242270665192, -30.71115380933863648, 102.9999999999999858 ) ) ;
#11611 = EDGE_CURVE ( 'NONE', #12372, #12231, #9529, .T. ) ;
#11612 = VECTOR ( 'NONE', #7233, 1000.000000000000000 ) ;
#11613 = CARTESIAN_POINT ( 'NONE',  ( 232.1454721953969056, -34.99999999999999289, 102.7245357809972290 ) ) ;
#11614 = CARTESIAN_POINT ( 'NONE',  ( 85.40000000000000568, -32.68124999877097281, -98.26794919243111792 ) ) ;
#11615 = CARTESIAN_POINT ( 'NONE',  ( 234.0999999999999375, -31.64999999999999858, 102.5980762113533018 ) ) ;
#11616 = EDGE_CURVE ( 'NONE', #2738, #12107, #9793, .T. ) ;
#11617 = ADVANCED_FACE ( 'NONE', ( #10082 ), #17125, .T. ) ;
#11618 = ORIENTED_EDGE ( 'NONE', *, *, #18431, .T. ) ;
#11619 = CARTESIAN_POINT ( 'NONE',  ( 232.5999999999999375, -34.55624999877095860, 97.00000000000000000 ) ) ;
#11620 = CARTESIAN_POINT ( 'NONE',  ( 234.0999999999999375, -32.49374999877096570, 102.5980762113533018 ) ) ;
#11621 = CARTESIAN_POINT ( 'NONE',  ( 231.0999999999999375, -34.06874999877096144, -52.59807621135342970 ) ) ;
#11622 = CARTESIAN_POINT ( 'NONE',  ( 229.5999999999999375, -32.68124999877096570, 98.26794919243111792 ) ) ;
#11623 = CARTESIAN_POINT ( 'NONE',  ( -83.77821517812500929, -32.01562499938548001, 97.61286128772489690 ) ) ;
#11624 = ORIENTED_EDGE ( 'NONE', *, *, #2917, .F. ) ;
#11625 = VERTEX_POINT ( 'NONE', #15854 ) ;
#11626 = CARTESIAN_POINT ( 'NONE',  ( -4.211140560182196957, 2.431303136016537803, -3.745885042887433514 ) ) ;
#11627 = COLOUR_RGB ( '',0.8941176470588234615, 0.8941176470588234615, 0.8941176470588234615 ) ;
#11628 =( BOUNDED_CURVE ( )  B_SPLINE_CURVE ( 2, ( #781, #7807, #16898, #13761, #13852, #2143, #15325, #399, #12490 ),
 .UNSPECIFIED., .F., .F. ) 
 B_SPLINE_CURVE_WITH_KNOTS ( ( 3, 2, 2, 2, 3 ),
 ( 0.6041666666666666297, 0.6111111111111111605, 0.6250000000000000000, 0.6388888888888888395, 0.6458333333333333703 ),
 .UNSPECIFIED. ) 
 CURVE ( )  GEOMETRIC_REPRESENTATION_ITEM ( )  RATIONAL_B_SPLINE_CURVE ( ( 0.9330127018922192983, 0.9330127018922187432, 1.000000000000000000, 0.8660254037844387076, 1.000000000000000000, 0.8660254037844387076, 1.000000000000000000, 0.9330127018922187432, 0.9330127018922192983 ) ) 
 REPRESENTATION_ITEM ( '' )  );
#11629 =( GEOMETRIC_REPRESENTATION_CONTEXT ( 3 ) GLOBAL_UNCERTAINTY_ASSIGNED_CONTEXT ( ( #17216 ) ) GLOBAL_UNIT_ASSIGNED_CONTEXT ( ( #16424, #17896, #16813 ) ) REPRESENTATION_CONTEXT ( 'NONE', 'WORKASPACE' ) );
#11630 = FACE_OUTER_BOUND ( 'NONE', #10819, .T. ) ;
#11631 = ORIENTED_EDGE ( 'NONE', *, *, #4099, .T. ) ;
#11632 = CARTESIAN_POINT ( 'NONE',  ( -85.40000000000000568, -31.78124999877096712, 98.26794919243111792 ) ) ;
#11633 = CARTESIAN_POINT ( 'NONE',  ( 85.40000000000000568, -31.80000000000000071, -99.99999999999998579 ) ) ;
#11634 = CARTESIAN_POINT ( 'NONE',  ( 82.39076102795760903, -31.99999999999999289, -102.8695224571928719 ) ) ;
#11635 = EDGE_CURVE ( 'NONE', #6898, #10655, #18685, .T. ) ;
#11636 = CARTESIAN_POINT ( 'NONE',  ( -79.64356964375001269, -32.24062499938548854, 98.40857419181659793 ) ) ;
#11637 = CARTESIAN_POINT ( 'NONE',  ( -82.39999999999999147, -32.81250000000000000, 96.53589838486223584 ) ) ;
#11638 = EDGE_CURVE ( 'NONE', #4516, #5783, #14783, .T. ) ;
#11639 = CARTESIAN_POINT ( 'NONE',  ( 232.5999999999999375, -32.30624999877096570, -53.00000000000011369 ) ) ;
#11640 = EDGE_CURVE ( 'NONE', #5588, #12381, #16789, .T. ) ;
#11641 = CARTESIAN_POINT ( 'NONE',  ( -84.69814130370966154, -35.19739829545387977, 98.07164667444374118 ) ) ;
#11642 = DIRECTION ( 'NONE',  ( -0.000000000000000000, -0.000000000000000000, -1.000000000000000000 ) ) ;
#11643 = VECTOR ( 'NONE', #16085, 1000.000000000000000 ) ;
#11644 = CARTESIAN_POINT ( 'NONE',  ( 229.8435696437499871, -30.17812499938547433, 98.40857419181659793 ) ) ;
#11645 = ORIENTED_EDGE ( 'NONE', *, *, #11202, .T. ) ;
#11646 = SURFACE_STYLE_USAGE ( .BOTH. , #4320 ) ;
#11647 = CARTESIAN_POINT ( 'NONE',  ( -79.64356964375001269, -30.85312499938548569, -98.40857419181659793 ) ) ;
#11648 = LINE ( 'NONE', #1013, #1180 ) ;
#11649 = CARTESIAN_POINT ( 'NONE',  ( -4.141042297810615835, 2.227970268150415656, -3.687027686973619822 ) ) ;
#11650 = CARTESIAN_POINT ( 'NONE',  ( 232.5999999999999943, -33.74062499938548143, 103.1828516163667899 ) ) ;
#11651 = CARTESIAN_POINT ( 'NONE',  ( -79.64356964375001269, -31.75312499938548427, 101.5914258081833879 ) ) ;
#11652 = CARTESIAN_POINT ( 'NONE',  ( 99.99999999999997158, -5.200000000000008171, -100.0000000000000000 ) ) ;
#11653 = CARTESIAN_POINT ( 'NONE',  ( 232.5999999999999375, -33.62812499938547717, -46.81714838363331666 ) ) ;
#11654 = ORIENTED_EDGE ( 'NONE', *, *, #10828, .F. ) ;
#11655 = VERTEX_POINT ( 'NONE', #3684 ) ;
#11656 = CARTESIAN_POINT ( 'NONE',  ( -79.64356964375001269, -34.45312499938548711, 101.5914258081833879 ) ) ;
#11657 = CARTESIAN_POINT ( 'NONE',  ( 79.39999999999999147, -30.63750000000000284, 101.7320508075688821 ) ) ;
#11658 = CARTESIAN_POINT ( 'NONE',  ( -69.99999999999998579, -32.00000000000000000, 150.0000000000000000 ) ) ;
#11659 = CARTESIAN_POINT ( 'NONE',  ( 235.3564303562499447, -31.26562499938547646, 99.99999999999998579 ) ) ;
#11660 = CARTESIAN_POINT ( 'NONE',  ( 82.40000000000000568, -32.30624999877097281, 102.9999999999999858 ) ) ;
#11661 = ADVANCED_FACE ( 'NONE', ( #4973 ), #9650, .T. ) ;
#11662 = ADVANCED_FACE ( 'NONE', ( #10914 ), #6530, .F. ) ;
#11663 = DIRECTION ( 'NONE',  ( 0.000000000000000000, -1.000000000000000000, -1.073081856240827827E-16 ) ) ;
#11664 = CARTESIAN_POINT ( 'NONE',  ( 81.02178482187500208, -33.59062499938548285, 97.61286128772489690 ) ) ;
#11665 = CARTESIAN_POINT ( 'NONE',  ( 79.64356964375001269, -30.77812499938548285, -98.40857419181659793 ) ) ;
#11666 = CARTESIAN_POINT ( 'NONE',  ( 235.3564303562499447, -34.37812499938547717, -51.59142580818350865 ) ) ;
#11667 = CARTESIAN_POINT ( 'NONE',  ( -81.02178482187500208, -34.34062499938548285, 97.61286128772489690 ) ) ;
#11668 = CARTESIAN_POINT ( 'NONE',  ( 82.39999999999999147, -31.60312499938548569, -96.81714838363319586 ) ) ;
#11669 = EDGE_LOOP ( 'NONE', ( #3236, #5010, #17084, #17900, #14839, #13874, #3326, #5301, #10473, #16480, #13253, #15367, #17207, #14833, #8198, #3069, #7711 ) ) ;
#11670 = CARTESIAN_POINT ( 'NONE',  ( 81.02178482187500208, -34.00312499938548427, 102.3871387122750889 ) ) ;
#11671 = CARTESIAN_POINT ( 'NONE',  ( -85.40000000000000568, -34.89374999877097139, 99.99999999999998579 ) ) ;
#11672 = EDGE_CURVE ( 'NONE', #3084, #7081, #12663, .T. ) ;
#11673 = CARTESIAN_POINT ( 'NONE',  ( 235.3564303562499447, -31.37812499938547717, -50.00000000000011369 ) ) ;
#11674 = CARTESIAN_POINT ( 'NONE',  ( -79.64356964375001269, -34.00312499938549138, 101.5914258081833879 ) ) ;
#11675 = EDGE_LOOP ( 'NONE', ( #330, #12342, #8137, #17972, #9463 ) ) ;
#11676 = CARTESIAN_POINT ( 'NONE',  ( -83.90000000000000568, -30.37500000000000355, 102.5980762113533018 ) ) ;
#11677 = CARTESIAN_POINT ( 'NONE',  ( 229.8435696437499587, -32.42812499938548143, 98.40857419181659793 ) ) ;
#11678 = PLANE ( 'NONE',  #3293 ) ;
#11679 = CARTESIAN_POINT ( 'NONE',  ( -80.90000000000000568, -31.94606250001229242, 97.40192378864668399 ) ) ;
#11680 = CARTESIAN_POINT ( 'NONE',  ( -81.59615242270665192, -34.81740381056767575, 103.0000000000000000 ) ) ;
#11681 = CARTESIAN_POINT ( 'NONE',  ( 231.4702054326072016, -32.00000000000000711, -47.41965524898115092 ) ) ;
#11682 = CARTESIAN_POINT ( 'NONE',  ( -83.77821517812500929, -31.41562499938548569, 102.3871387122750889 ) ) ;
#11683 = CARTESIAN_POINT ( 'NONE',  ( 230.7186334667983658, -32.00000000000000711, 97.98546077809203325 ) ) ;
#11684 = CARTESIAN_POINT ( 'NONE',  ( 85.15643035624999868, -32.01562499938548711, 98.40857419181659793 ) ) ;
#11685 = CARTESIAN_POINT ( 'NONE',  ( 0.02944718078426969768, -0.6813962075686098574, 3.500000000000000888 ) ) ;
#11686 = CARTESIAN_POINT ( 'NONE',  ( 83.77821517812500929, -32.87812499938548427, -102.3871387122750889 ) ) ;
#11687 = CARTESIAN_POINT ( 'NONE',  ( -83.77821517812500929, -32.42812499938548854, -97.61286128772489690 ) ) ;
#11688 = ORIENTED_EDGE ( 'NONE', *, *, #17389, .T. ) ;
#11689 = CARTESIAN_POINT ( 'NONE',  ( 79.39999999999999147, -33.80624999877097281, 98.26794919243113213 ) ) ;
#11690 = CARTESIAN_POINT ( 'NONE',  ( 232.5999999999999375, -34.86562499938548143, 96.81714838363319586 ) ) ;
#11691 = CARTESIAN_POINT ( 'NONE',  ( 235.3564303562499447, -34.49062499938548143, -51.59142580818350865 ) ) ;
#11692 = CARTESIAN_POINT ( 'NONE',  ( -85.15643035625001289, -30.25312499938548783, 99.99999999999998579 ) ) ;
#11693 = DIRECTION ( 'NONE',  ( 1.000000000000000000, 0.000000000000000000, 0.000000000000000000 ) ) ;
#11694 = VERTEX_POINT ( 'NONE', #5260 ) ;
#11695 = CARTESIAN_POINT ( 'NONE',  ( -79.64356964375001269, -34.37812499938548427, -101.5914258081833879 ) ) ;
#11696 = CARTESIAN_POINT ( 'NONE',  ( 4.000000000000000000, -1.700175430507292473, -3.320327275037661785 ) ) ;
#11697 = VERTEX_POINT ( 'NONE', #3484 ) ;
#11698 = CARTESIAN_POINT ( 'NONE',  ( 229.5999999999999375, -33.56249999999999289, -48.26794919243123161 ) ) ;
#11699 = CARTESIAN_POINT ( 'NONE',  ( -82.39999999999999147, -30.81562499938548427, -103.1828516163667899 ) ) ;
#11700 = CARTESIAN_POINT ( 'NONE',  ( -80.07765479359939320, -32.00000000000000711, -101.8487127466165845 ) ) ;
#11701 = CARTESIAN_POINT ( 'NONE',  ( -82.39999999999999147, -31.63124999877097210, -96.53589838486223584 ) ) ;
#11702 = CARTESIAN_POINT ( 'NONE',  ( 229.8435696437499871, -32.54062499938547859, 98.40857419181659793 ) ) ;
#11703 = CARTESIAN_POINT ( 'NONE',  ( -79.39999999999999147, -30.62268749875867968, 99.99999999999998579 ) ) ;
#11704 = ADVANCED_FACE ( 'NONE', ( #15508 ), #13937, .F. ) ;
#11705 = CARTESIAN_POINT ( 'NONE',  ( -83.77821517812500929, -33.92812499938548854, 97.61286128772489690 ) ) ;
#11706 = CARTESIAN_POINT ( 'NONE',  ( -83.77821517812500929, -34.56562499938548427, -97.61286128772489690 ) ) ;
#11707 = PLANE ( 'NONE',  #274 ) ;
#11708 = AXIS2_PLACEMENT_3D ( 'NONE', #4280, #5942, #17478 ) ;
#11709 = DIRECTION ( 'NONE',  ( -1.000000000000000000, -0.000000000000000000, -0.000000000000000000 ) ) ;
#11710 = CARTESIAN_POINT ( 'NONE',  ( 79.39999999999999147, -32.86874999877097281, -99.99999999999998579 ) ) ;
#11711 = CARTESIAN_POINT ( 'NONE',  ( 229.5999999999999375, -32.28750000000000142, 98.26794919243111792 ) ) ;
#11712 = ORIENTED_EDGE ( 'NONE', *, *, #18566, .F. ) ;
#11713 = DIRECTION ( 'NONE',  ( -1.000000000000000000, 0.000000000000000000, 0.000000000000000000 ) ) ;
#11714 = B_SPLINE_CURVE_WITH_KNOTS ( 'NONE', 3,
 ( #7729, #12221, #3428, #5097, #9479, #10753, #3230, #11041, #15442, #420, #9285, #18384, #6461, #9189, #15545, #2054 ),
 .UNSPECIFIED., .F., .F.,
 ( 4, 3, 3, 3, 3, 4 ),
 ( 0.000000000000000000, 3.315506744709139969E-05, 6.608280158700174001E-05, 0.0001026520855292366530, 0.0001376952025668715498, 0.0001398064759194521725 ),
 .UNSPECIFIED. ) ;
#11715 = CARTESIAN_POINT ( 'NONE',  ( 232.5999999999999375, -31.85624999877096641, 96.53589838486223584 ) ) ;
#11716 = CARTESIAN_POINT ( 'NONE',  ( 235.5999999999999943, -34.25624999877096855, -48.26794919243124582 ) ) ;
#11717 = CARTESIAN_POINT ( 'NONE',  ( -81.02178482187500208, -34.04062499938548569, 102.3871387122750889 ) ) ;
#11718 = EDGE_LOOP ( 'NONE', ( #7322, #11645, #5390, #583 ) ) ;
#11719 = EDGE_LOOP ( 'NONE', ( #8473, #6238, #18911, #6416 ) ) ;
#11720 = VECTOR ( 'NONE', #8842, 1000.000000000000000 ) ;
#11721 = CYLINDRICAL_SURFACE ( 'NONE', #12227, 7.000000000000006217 ) ;
#11722 = CARTESIAN_POINT ( 'NONE',  ( -82.40000000000000568, -32.08124999877097139, 102.9999999999999858 ) ) ;
#11723 = ORIENTED_EDGE ( 'NONE', *, *, #19273, .T. ) ;
#11724 = CARTESIAN_POINT ( 'NONE',  ( 80.90000000000000568, -32.49374999877097281, -102.5980762113533018 ) ) ;
#11725 = CARTESIAN_POINT ( 'NONE',  ( 79.39999999999999147, -34.23750000000000426, -98.26794919243110371 ) ) ;
#11726 = CARTESIAN_POINT ( 'NONE',  ( 244.7999999999999545, -35.00000000000000000, -97.80000000000002558 ) ) ;
#11727 = EDGE_CURVE ( 'NONE', #10663, #138, #8078, .T. ) ;
#11728 = CARTESIAN_POINT ( 'NONE',  ( -85.15643035624999868, -33.81562499938549138, 101.5914258081833879 ) ) ;
#11729 = CARTESIAN_POINT ( 'NONE',  ( -82.39999999999999147, -31.91250000000000497, 96.53589838486223584 ) ) ;
#11730 = CARTESIAN_POINT ( 'NONE',  ( 235.5999999999999943, -32.45624999877096428, -48.26794919243124582 ) ) ;
#11731 = CARTESIAN_POINT ( 'NONE',  ( 99.99999999999998579, 0.000000000000000000, -150.0000000000000000 ) ) ;
#11732 =( GEOMETRIC_REPRESENTATION_CONTEXT ( 3 ) GLOBAL_UNCERTAINTY_ASSIGNED_CONTEXT ( ( #5102 ) ) GLOBAL_UNIT_ASSIGNED_CONTEXT ( ( #14163, #1175, #8586 ) ) REPRESENTATION_CONTEXT ( 'NONE', 'WORKASPACE' ) );
#11733 = CARTESIAN_POINT ( 'NONE',  ( 105.1999999999999744, -34.99999999999999289, -100.0000000000000000 ) ) ;
#11734 = CARTESIAN_POINT ( 'NONE',  ( 0.1388410611046087539, 3.710337782248032568, 0.5735064479039790886 ) ) ;
#11735 = AXIS2_PLACEMENT_3D ( 'NONE', #5970, #8985, #16418 ) ;
#11736 = CARTESIAN_POINT ( 'NONE',  ( -82.40000000000000568, -34.38749999999999574, -96.99999999999998579 ) ) ;
#11737 = VERTEX_POINT ( 'NONE', #1239 ) ;
#11738 = DIRECTION ( 'NONE',  ( 1.000000000000000000, 0.000000000000000000, 0.000000000000000000 ) ) ;
#11739 = CARTESIAN_POINT ( 'NONE',  ( -83.77821517812500929, -35.12812499938548427, -97.61286128772489690 ) ) ;
#11740 = CARTESIAN_POINT ( 'NONE',  ( 235.5999999999999943, -33.35624999877096286, -48.26794919243124582 ) ) ;
#11741 = ADVANCED_FACE ( 'NONE', ( #4169, #19212, #9937 ), #14701, .T. ) ;
#11742 = DIRECTION ( 'NONE',  ( 1.000000000000000000, -4.970554372426382520E-17, -0.000000000000000000 ) ) ;
#11743 = CARTESIAN_POINT ( 'NONE',  ( 1.567478505476134606E-15, 4.618802153517012066, -3.433295621305382905 ) ) ;
#11744 = CARTESIAN_POINT ( 'NONE',  ( -85.15643035625001289, -30.59062499938548285, 99.99999999999998579 ) ) ;
#11745 = CARTESIAN_POINT ( 'NONE',  ( 81.59615242270665192, -33.28259618943233278, 103.0000000000000000 ) ) ;
#11746 = CARTESIAN_POINT ( 'NONE',  ( 233.9782151781249411, -31.79062499938548214, -47.61286128772501769 ) ) ;
#11747 = ORIENTED_EDGE ( 'NONE', *, *, #12505, .F. ) ;
#11748 = ORIENTED_EDGE ( 'NONE', *, *, #4504, .F. ) ;
#11749 = FACE_OUTER_BOUND ( 'NONE', #10352, .T. ) ;
#11750 = CARTESIAN_POINT ( 'NONE',  ( -79.39999999999999147, -32.02500000000000568, 99.99999999999998579 ) ) ;
#11751 = EDGE_CURVE ( 'NONE', #6735, #6176, #4578, .T. ) ;
#11752 = CARTESIAN_POINT ( 'NONE',  ( -81.59615242270662350, -33.91740381056766296, -96.99999999999997158 ) ) ;
#11753 = CARTESIAN_POINT ( 'NONE',  ( 83.77821517812500929, -34.26562499938548711, 102.3871387122750889 ) ) ;
#11754 = LINE ( 'NONE', #2864, #5877 ) ;
#11755 = CARTESIAN_POINT ( 'NONE',  ( 229.8435696437499303, -31.94062499938547717, 99.99999999999998579 ) ) ;
#11756 = CARTESIAN_POINT ( 'NONE',  ( 229.8435696437499587, -33.77812499938547575, -51.59142580818350154 ) ) ;
#11757 = CARTESIAN_POINT ( 'NONE',  ( -81.59615242270662350, -33.73259618943233562, 96.99999999999998579 ) ) ;
#11758 = CARTESIAN_POINT ( 'NONE',  ( 79.64356964375001269, -34.90312499938548285, 98.40857419181659793 ) ) ;
#11759 = CARTESIAN_POINT ( 'NONE',  ( 82.39999999999999147, -31.15312499938548640, -96.81714838363319586 ) ) ;
#11760 = CARTESIAN_POINT ( 'NONE',  ( 235.5999999999999943, -31.08749999999999503, -51.73205080756900287 ) ) ;
#11761 = CARTESIAN_POINT ( 'NONE',  ( 83.77821517812500929, -32.46562499938548285, -97.61286128772489690 ) ) ;
#11762 = AXIS2_PLACEMENT_3D ( 'NONE', #10298, #6172, #16711 ) ;
#11763 = ORIENTED_EDGE ( 'NONE', *, *, #18919, .T. ) ;
#11764 = CARTESIAN_POINT ( 'NONE',  ( 82.39999999999999147, -34.86562499938548854, 103.1828516163667899 ) ) ;
#11765 = LINE ( 'NONE', #10494, #886 ) ;
#11766 = CARTESIAN_POINT ( 'NONE',  ( 231.2217848218749339, -31.97812499938548214, -47.61286128772501769 ) ) ;
#11767 = CARTESIAN_POINT ( 'NONE',  ( -81.02178482187500208, -32.99062499938548854, 97.61286128772489690 ) ) ;
#11768 = ORIENTED_EDGE ( 'NONE', *, *, #13046, .F. ) ;
#11769 = CARTESIAN_POINT ( 'NONE',  ( -84.75088379146899342, -35.00000000000000711, 101.6079878054202652 ) ) ;
#11770 = AXIS2_PLACEMENT_3D ( 'NONE', #13087, #15929, #5489 ) ;
#11771 = CARTESIAN_POINT ( 'NONE',  ( 4.175813232069146785, 2.061359961916366057, -3.570380186727397653 ) ) ;
#11772 = CARTESIAN_POINT ( 'NONE',  ( 230.2961164517930968, -35.00002705695767702, -51.92148140967023551 ) ) ;
#11773 = CARTESIAN_POINT ( 'NONE',  ( -82.39999999999999147, -32.35856250001229739, 96.53589838486223584 ) ) ;
#11774 = VECTOR ( 'NONE', #8512, 1000.000000000000000 ) ;
#11775 = VECTOR ( 'NONE', #11357, 1000.000000000000000 ) ;
#11776 = CARTESIAN_POINT ( 'NONE',  ( -3.333333333333335258, 2.694301256218251783, -3.300726591567079815 ) ) ;
#11777 = EDGE_CURVE ( 'NONE', #8755, #6484, #833, .T. ) ;
#11778 = LINE ( 'NONE', #6115, #5250 ) ;
#11779 = CARTESIAN_POINT ( 'NONE',  ( -82.39999999999999147, -31.60312499938548569, 96.81714838363319586 ) ) ;
#11780 = CARTESIAN_POINT ( 'NONE',  ( -83.20384757729337366, -32.55134618820330417, 103.0000000000000000 ) ) ;
#11781 = CARTESIAN_POINT ( 'NONE',  ( 82.39999999999999147, -31.49062499938548854, 96.81714838363319586 ) ) ;
#11782 = CARTESIAN_POINT ( 'NONE',  ( 113.0000000000000142, 10.39615242270647144, 50.00000000000001421 ) ) ;
#11783 = VECTOR ( 'NONE', #1769, 1000.000000000000000 ) ;
#11784 = CARTESIAN_POINT ( 'NONE',  ( 244.7999999999999545, -4.999999999999976907, 153.0000000000000000 ) ) ;
#11785 = CARTESIAN_POINT ( 'NONE',  ( -85.15643035625001289, -32.09062499938548996, 98.40857419181659793 ) ) ;
#11786 = CARTESIAN_POINT ( 'NONE',  ( -83.77821517812500929, -31.52812499938548996, -97.61286128772489690 ) ) ;
#11787 = EDGE_LOOP ( 'NONE', ( #16378, #15650, #9777, #1732, #14430 ) ) ;
#11788 = CARTESIAN_POINT ( 'NONE',  ( 80.90000000000000568, -34.29374999877096997, 97.40192378864668399 ) ) ;
#11789 = DIRECTION ( 'NONE',  ( 0.000000000000000000, 0.000000000000000000, -1.000000000000000000 ) ) ;
#11790 = DIRECTION ( 'NONE',  ( -0.000000000000000000, 0.000000000000000000, -1.000000000000000000 ) ) ;
#11791 = AXIS2_PLACEMENT_3D ( 'NONE', #13426, #7561, #17926 ) ;
#11792 = AXIS2_PLACEMENT_3D ( 'NONE', #6888, #16587, #12838 ) ;
#11793 = CARTESIAN_POINT ( 'NONE',  ( -81.02178482187500208, -31.00312499938548783, 102.3871387122750889 ) ) ;
#11794 = CARTESIAN_POINT ( 'NONE',  ( 80.07765479365677663, -31.99999999999999289, 101.8487127466820965 ) ) ;
#11795 = ORIENTED_EDGE ( 'NONE', *, *, #18843, .T. ) ;
#11796 = CARTESIAN_POINT ( 'NONE',  ( -85.15643035624999868, -34.60312499938548569, -98.40857419181659793 ) ) ;
#11797 = DIRECTION ( 'NONE',  ( 0.000000000000000000, -1.261617073437673828E-14, -1.000000000000000000 ) ) ;
#11798 = VERTEX_POINT ( 'NONE', #2796 ) ;
#11799 = ADVANCED_FACE ( 'NONE', ( #11588 ), #10222, .T. ) ;
#11800 = CARTESIAN_POINT ( 'NONE',  ( 231.0999999999999375, -33.52499999999999147, -47.40192378864679768 ) ) ;
#11801 = AXIS2_PLACEMENT_3D ( 'NONE', #16915, #9482, #6563 ) ;
#11802 = CARTESIAN_POINT ( 'NONE',  ( -81.02178482187500208, -32.65312499938548996, -102.3871387122750889 ) ) ;
#11803 = CARTESIAN_POINT ( 'NONE',  ( -94.79999999999999716, -5.200000000000000178, -150.0000000000000000 ) ) ;
#11804 = CARTESIAN_POINT ( 'NONE',  ( -85.40000000000000568, -32.23124999877096997, -101.7320508075688679 ) ) ;
#11805 = CARTESIAN_POINT ( 'NONE',  ( 235.3564303562499447, -32.72812499938547859, 99.99999999999998579 ) ) ;
#11806 = CARTESIAN_POINT ( 'NONE',  ( -79.39999999999999147, -31.03518749875868110, 98.26794919243110371 ) ) ;
#11807 = CARTESIAN_POINT ( 'NONE',  ( -79.64356964375001269, -32.69062499938548427, 98.40857419181659793 ) ) ;
#11808 = CONICAL_SURFACE ( 'NONE', #18987, 2.500000000000000888, 0.9599310885968785900 ) ;
#11809 = CARTESIAN_POINT ( 'NONE',  ( -83.90000000000000568, -33.61874999877097281, 97.40192378864668399 ) ) ;
#11810 = DIRECTION ( 'NONE',  ( 0.000000000000000000, 0.000000000000000000, 1.000000000000000000 ) ) ;
#11811 = CARTESIAN_POINT ( 'NONE',  ( -82.40000000000000568, -33.03750000000000142, 102.9999999999999858 ) ) ;
#11812 = CARTESIAN_POINT ( 'NONE',  ( 80.90000000000000568, -32.34374999877096712, -97.40192378864668399 ) ) ;
#11813 = CARTESIAN_POINT ( 'NONE',  ( 234.0999999999999375, -34.64999999999999147, 97.40192378864668399 ) ) ;
#11814 = EDGE_LOOP ( 'NONE', ( #8046, #11011, #2161, #17738, #6352, #3307, #13308, #1873, #1399, #14071, #7969, #15132, #2122, #3930, #3426, #14548, #13182 ) ) ;
#11815 = CARTESIAN_POINT ( 'NONE',  ( 235.5999999999999943, -34.63124999877096144, 98.26794919243110371 ) ) ;
#11816 = CARTESIAN_POINT ( 'NONE',  ( 231.0999999999999375, -34.96874999877096002, 97.40192378864668399 ) ) ;
#11817 = CARTESIAN_POINT ( 'NONE',  ( 232.5999999999999375, -34.55624999877095860, -53.46410161513786363 ) ) ;
#11818 = CARTESIAN_POINT ( 'NONE',  ( -81.02178482187500208, -34.34062499938548285, 97.61286128772489690 ) ) ;
#11819 = ORIENTED_EDGE ( 'NONE', *, *, #2828, .F. ) ;
#11820 = VERTEX_POINT ( 'NONE', #3874 ) ;
#11821 = CARTESIAN_POINT ( 'NONE',  ( -82.61711639273519836, -31.99999999999998579, 97.16008101253264329 ) ) ;
#11822 = CARTESIAN_POINT ( 'NONE',  ( 99.99999999999997158, -5.200000000000008171, 150.0000000000000000 ) ) ;
#11823 = CARTESIAN_POINT ( 'NONE',  ( -83.20384757729335945, -32.28615380933863577, 97.00000000000000000 ) ) ;
#11824 = ORIENTED_EDGE ( 'NONE', *, *, #15198, .T. ) ;
#11825 = CARTESIAN_POINT ( 'NONE',  ( -80.17984880387896851, -35.00000000000000000, 101.6434491389460959 ) ) ;
#11826 = CARTESIAN_POINT ( 'NONE',  ( -1.149515148933662080E-15, -4.736529461166056443, -3.681130640444383317 ) ) ;
#11827 = B_SPLINE_CURVE_WITH_KNOTS ( 'NONE', 3,
 ( #18414, #9514, #10974, #12354, #15480, #2282 ),
 .UNSPECIFIED., .F., .F.,
 ( 4, 2, 4 ),
 ( 0.000000000000000000, 0.002086519881787259317, 0.004173039763574518633 ),
 .UNSPECIFIED. ) ;
#11828 = CARTESIAN_POINT ( 'NONE',  ( -82.39999999999999147, -33.51562499938548001, 96.81714838363319586 ) ) ;
#11829 = CARTESIAN_POINT ( 'NONE',  ( -79.39999999999999147, -32.96250000000000568, 101.7320508075688537 ) ) ;
#11830 = CARTESIAN_POINT ( 'NONE',  ( -85.40000000000000568, -30.88124999877097210, 98.26794919243111792 ) ) ;
#11831 = DIRECTION ( 'NONE',  ( 0.000000000000000000, 0.000000000000000000, 1.000000000000000000 ) ) ;
#11832 = FACE_OUTER_BOUND ( 'NONE', #3581, .T. ) ;
#11833 = CARTESIAN_POINT ( 'NONE',  ( -81.48596794228828344, -35.00000000000000711, -102.8136019330778339 ) ) ;
#11834 = CARTESIAN_POINT ( 'NONE',  ( -83.90000000000000568, -34.57500000000000284, -102.5980762113533018 ) ) ;
#11835 = ORIENTED_EDGE ( 'NONE', *, *, #6983, .F. ) ;
#11836 = CARTESIAN_POINT ( 'NONE',  ( -85.15643035625001289, -31.04062499938548569, -99.99999999999998579 ) ) ;
#11837 = DIRECTION ( 'NONE',  ( -0.7071067811865505703, 8.659560562354895880E-17, -0.7071067811865444641 ) ) ;
#11838 = LINE ( 'NONE', #4416, #14878 ) ;
#11839 = DIRECTION ( 'NONE',  ( -0.000000000000000000, -0.000000000000000000, -1.000000000000000000 ) ) ;
#11840 = CARTESIAN_POINT ( 'NONE',  ( -81.02178482187500208, -32.09062499938548285, 97.61286128772489690 ) ) ;
#11841 = CARTESIAN_POINT ( 'NONE',  ( 232.5999999999999375, -29.99999999999999645, 99.99999999999998579 ) ) ;
#11842 = CARTESIAN_POINT ( 'NONE',  ( 235.3564303562499447, -31.75312499938547717, -48.40857419181671162 ) ) ;
#11843 = ORIENTED_EDGE ( 'NONE', *, *, #8093, .F. ) ;
#11844 = ORIENTED_EDGE ( 'NONE', *, *, #1712, .T. ) ;
#11845 = CARTESIAN_POINT ( 'NONE',  ( -82.40000000000000568, -31.68750000000000711, 102.9999999999999858 ) ) ;
#11846 = CARTESIAN_POINT ( 'NONE',  ( -79.39999999999999147, -31.53750000000000497, 98.26794919243110371 ) ) ;
#11847 = CARTESIAN_POINT ( 'NONE',  ( -80.90000000000000568, -31.14374999877097139, 102.5980762113533018 ) ) ;
#11848 = CARTESIAN_POINT ( 'NONE',  ( 79.39999999999999147, -32.47500000000000142, 99.99999999999998579 ) ) ;
#11849 = CARTESIAN_POINT ( 'NONE',  ( -4.211140560182196957, 2.431303136016537803, -3.745885042887433514 ) ) ;
#11850 = CARTESIAN_POINT ( 'NONE',  ( 231.2217848218749339, -33.21562499938547575, 102.3871387122750889 ) ) ;
#11851 = CARTESIAN_POINT ( 'NONE',  ( 235.3564303562499447, -33.51562499938548001, -50.00000000000011369 ) ) ;
#11852 = CARTESIAN_POINT ( 'NONE',  ( 84.51154815724953551, -35.14114861271051637, 101.7717992799616553 ) ) ;
#11853 =( BOUNDED_CURVE ( )  B_SPLINE_CURVE ( 2, ( #8728, #5997, #11949, #19093, #5714, #4242, #15966, #8535, #14484 ),
 .UNSPECIFIED., .F., .F. ) 
 B_SPLINE_CURVE_WITH_KNOTS ( ( 3, 2, 2, 2, 3 ),
 ( 0.4791666666666666297, 0.4861111111111111049, 0.5000000000000000000, 0.5138888888888888395, 0.5208333333333334814 ),
 .UNSPECIFIED. ) 
 CURVE ( )  GEOMETRIC_REPRESENTATION_ITEM ( )  RATIONAL_B_SPLINE_CURVE ( ( 0.9330127018922194093, 0.9330127018922190762, 1.000000000000000000, 0.8660254037844387076, 1.000000000000000000, 0.8660254037844387076, 1.000000000000000000, 0.9330127018922177440, 0.9330127018922194093 ) ) 
 REPRESENTATION_ITEM ( '' )  );
#11854 = CARTESIAN_POINT ( 'NONE',  ( 85.15643035624999868, -32.42812499938548854, -98.40857419181659793 ) ) ;
#11855 = CARTESIAN_POINT ( 'NONE',  ( 233.9782151781249411, -34.49062499938548143, -47.61286128772501769 ) ) ;
#11856 = CARTESIAN_POINT ( 'NONE',  ( 82.40000000000000568, -30.00000000000000355, -99.99999999999998579 ) ) ;
#11857 = CARTESIAN_POINT ( 'NONE',  ( 79.64356964375001269, -33.92812499938548854, -98.40857419181659793 ) ) ;
#11858 = EDGE_CURVE ( 'NONE', #12080, #11529, #7285, .T. ) ;
#11859 = ORIENTED_EDGE ( 'NONE', *, *, #8651, .T. ) ;
#11860 = CARTESIAN_POINT ( 'NONE',  ( 82.40000000000000568, -30.00000000000000355, 99.99999999999998579 ) ) ;
#11861 = DIRECTION ( 'NONE',  ( -0.000000000000000000, 1.000000000000000000, -0.000000000000000000 ) ) ;
#11862 = CARTESIAN_POINT ( 'NONE',  ( 232.5999999999999375, -31.49062499938547788, -46.81714838363331666 ) ) ;
#11863 = CARTESIAN_POINT ( 'NONE',  ( -85.40000000000000568, -31.38749999999999574, 98.26794919243111792 ) ) ;
#11864 = VERTEX_POINT ( 'NONE', #13140 ) ;
#11865 = CARTESIAN_POINT ( 'NONE',  ( -80.90000000000000568, -33.00000000000000000, 102.5980762113533018 ) ) ;
#11866 = CARTESIAN_POINT ( 'NONE',  ( -81.59615242270662350, -30.97634618820330488, 96.99999999999998579 ) ) ;
#11867 = DIRECTION ( 'NONE',  ( -1.000000000000000000, 0.000000000000000000, 0.000000000000000000 ) ) ;
#11868 = CARTESIAN_POINT ( 'NONE',  ( -79.39999999999999147, -31.53356250001228744, 98.26794919243110371 ) ) ;
#11869 = EDGE_CURVE ( 'NONE', #4397, #3695, #18793, .T. ) ;
#11870 = CARTESIAN_POINT ( 'NONE',  ( -0.6666666666666651864, 4.233901974057260098, -3.300726591567081147 ) ) ;
#11871 = CARTESIAN_POINT ( 'NONE',  ( 231.9083760470965103, -32.00000000000000711, -47.24830349208670555 ) ) ;
#11872 = CARTESIAN_POINT ( 'NONE',  ( -85.15643035624999868, -31.52812499938547930, 98.40857419181659793 ) ) ;
#11873 = CARTESIAN_POINT ( 'NONE',  ( 85.11512745526613344, -31.99999999999998579, 99.40473233008030718 ) ) ;
#11874 = CARTESIAN_POINT ( 'NONE',  ( 83.77821517812500929, -32.12812499938548427, 102.3871387122750889 ) ) ;
#11875 = EDGE_CURVE ( 'NONE', #4909, #1155, #9305, .T. ) ;
#11876 = CARTESIAN_POINT ( 'NONE',  ( 244.7999999999999545, -5.000000000000000888, -103.0000000000000995 ) ) ;
#11877 = DIRECTION ( 'NONE',  ( 1.000000000000000000, 0.000000000000000000, 0.000000000000000000 ) ) ;
#11878 = CARTESIAN_POINT ( 'NONE',  ( -85.15643035625001289, -32.91562499938548569, 101.5914258081833879 ) ) ;
#11879 = CARTESIAN_POINT ( 'NONE',  ( -82.39999999999999147, -31.71562499938548640, -103.1828516163667899 ) ) ;
#11880 = ORIENTED_EDGE ( 'NONE', *, *, #925, .F. ) ;
#11881 = CARTESIAN_POINT ( 'NONE',  ( 85.40000000000000568, -35.36739044046696279, 101.0919052301551204 ) ) ;
#11882 = CARTESIAN_POINT ( 'NONE',  ( 82.39999999999999147, -34.33124999877097139, 97.00000000000000000 ) ) ;
#11883 = LINE ( 'NONE', #79, #14278 ) ;
#11884 = CARTESIAN_POINT ( 'NONE',  ( -85.15643035624999868, -31.64062499938548356, 98.40857419181659793 ) ) ;
#11885 = CARTESIAN_POINT ( 'NONE',  ( -85.32499745258149915, -35.00000000000000711, -100.1587029275224978 ) ) ;
#11886 = ORIENTED_EDGE ( 'NONE', *, *, #18798, .F. ) ;
#11887 = EDGE_CURVE ( 'NONE', #14762, #14362, #6446, .T. ) ;
#11888 = CARTESIAN_POINT ( 'NONE',  ( -82.39999999999999147, -33.62812499938549138, -96.81714838363319586 ) ) ;
#11889 = CARTESIAN_POINT ( 'NONE',  ( 4.158807179406255550, 2.089320655794525639, -3.500000000000000000 ) ) ;
#11890 = DIRECTION ( 'NONE',  ( 1.000000000000000000, 0.000000000000000000, -0.000000000000000000 ) ) ;
#11891 = CARTESIAN_POINT ( 'NONE',  ( -85.15643035624999868, -32.54062499938548569, -101.5914258081833879 ) ) ;
#11892 = DIRECTION ( 'NONE',  ( -0.000000000000000000, -1.000000000000000000, -0.000000000000000000 ) ) ;
#11893 = CARTESIAN_POINT ( 'NONE',  ( -82.39999999999999147, -30.95624999877097139, -103.4641016151377499 ) ) ;
#11894 = CARTESIAN_POINT ( 'NONE',  ( 231.2217848218749339, -31.67812499938547788, 97.61286128772489690 ) ) ;
#11895 = CARTESIAN_POINT ( 'NONE',  ( -79.39999999999999147, -32.46018749875867826, 101.7320508075688537 ) ) ;
#11896 = CARTESIAN_POINT ( 'NONE',  ( -82.39999999999999147, -33.06562499938548427, 96.81714838363319586 ) ) ;
#11897 = CARTESIAN_POINT ( 'NONE',  ( -79.64356964374999848, -34.41562499938548569, -99.99999999999998579 ) ) ;
#11898 = CARTESIAN_POINT ( 'NONE',  ( 79.64356964374998427, -34.00312499938548427, 98.40857419181659793 ) ) ;
#11899 = CARTESIAN_POINT ( 'NONE',  ( 81.59615242270662350, -32.38259618943233420, -96.99999999999998579 ) ) ;
#11900 =( BOUNDED_CURVE ( )  B_SPLINE_CURVE ( 2, ( #151, #17736, #10490, #4436, #10394, #2966, #16454, #17923, #3063 ),
 .UNSPECIFIED., .F., .F. ) 
 B_SPLINE_CURVE_WITH_KNOTS ( ( 3, 2, 2, 2, 3 ),
 ( 0.6875000000000000000, 0.6944444444444444198, 0.7083333333333333703, 0.7222222222222222099, 0.7291666666666666297 ),
 .UNSPECIFIED. ) 
 CURVE ( )  GEOMETRIC_REPRESENTATION_ITEM ( )  RATIONAL_B_SPLINE_CURVE ( ( 0.9330127018922194093, 0.9330127018922194093, 1.000000000000000000, 0.8660254037844387076, 1.000000000000000000, 0.8660254037844387076, 1.000000000000000000, 0.9330127018922198534, 0.9330127018922192983 ) ) 
 REPRESENTATION_ITEM ( '' )  );
#11901 = CARTESIAN_POINT ( 'NONE',  ( 235.5999999999999943, -33.28124999877096002, 98.26794919243110371 ) ) ;
#11902 = EDGE_CURVE ( 'NONE', #2874, #6898, #11446, .T. ) ;
#11903 = CARTESIAN_POINT ( 'NONE',  ( 82.39999999999999147, -34.78124999877096712, -103.4641016151377499 ) ) ;
#11904 = CARTESIAN_POINT ( 'NONE',  ( 235.5999999999999375, -33.82499999999999574, 99.99999999999998579 ) ) ;
#11905 = ORIENTED_EDGE ( 'NONE', *, *, #2920, .F. ) ;
#11906 = CARTESIAN_POINT ( 'NONE',  ( 85.15643035625001289, -34.60312499938548569, -101.5914258081833879 ) ) ;
#11907 = CARTESIAN_POINT ( 'NONE',  ( 234.0999999999999375, -35.04374999877096286, 97.40192378864668399 ) ) ;
#11908 = CARTESIAN_POINT ( 'NONE',  ( 231.0999999999999375, -32.71874999877096002, -52.59807621135342970 ) ) ;
#11909 = CARTESIAN_POINT ( 'NONE',  ( -79.64356964374998427, -34.45312499938548711, 101.5914258081833879 ) ) ;
#11910 = ORIENTED_EDGE ( 'NONE', *, *, #9832, .T. ) ;
#11912 = EDGE_LOOP ( 'NONE', ( #4768, #12001, #13449, #11171 ) ) ;
#11911 = EDGE_CURVE ( 'NONE', #18754, #14350, #6759, .T. ) ;
#11913 = PRODUCT_DEFINITION ( 'UNKNOWN', '', #3950, #9230 ) ;
#11914 = CARTESIAN_POINT ( 'NONE',  ( -4.000000000000000000, 0.8576368993457507139, -3.433240632782198709 ) ) ;
#11915 = CARTESIAN_POINT ( 'NONE',  ( -82.40000000000000568, -30.00000000000000355, -96.99999999999998579 ) ) ;
#11916 = EDGE_LOOP ( 'NONE', ( #12698, #18356, #2323 ) ) ;
#11917 = CARTESIAN_POINT ( 'NONE',  ( 105.1999999999999886, -29.79999999999999361, -100.0000000000000000 ) ) ;
#11918 = CARTESIAN_POINT ( 'NONE',  ( 82.40000000000000568, -31.99999999999999289, -99.99999999999998579 ) ) ;
#11919 = AXIS2_PLACEMENT_3D ( 'NONE', #954, #13928, #3677 ) ;
#11920 = VECTOR ( 'NONE', #11140, 1000.000000000000000 ) ;
#11921 = CARTESIAN_POINT ( 'NONE',  ( -79.64356964375001269, -35.01562499938548711, 101.5914258081833879 ) ) ;
#11922 = CARTESIAN_POINT ( 'NONE',  ( -80.90000000000000568, -34.20000000000000284, 97.40192378864668399 ) ) ;
#11923 = CARTESIAN_POINT ( 'NONE',  ( -85.40000000000000568, -31.29374999877096997, 99.99999999999998579 ) ) ;
#11924 = CYLINDRICAL_SURFACE ( 'NONE', #14129, 3.000000000000002665 ) ;
#11925 = DIRECTION ( 'NONE',  ( 0.000000000000000000, 0.000000000000000000, 1.000000000000000000 ) ) ;
#11926 = CARTESIAN_POINT ( 'NONE',  ( -82.40000000000001990, -33.26250000000000284, -103.0000000000000000 ) ) ;
#11927 = CARTESIAN_POINT ( 'NONE',  ( -80.48808202378404530, -35.00000000000000000, -102.1951992292040075 ) ) ;
#11928 = DIRECTION ( 'NONE',  ( 0.000000000000000000, 0.000000000000000000, 1.000000000000000000 ) ) ;
#11929 = VERTEX_POINT ( 'NONE', #17938 ) ;
#11930 = CARTESIAN_POINT ( 'NONE',  ( -83.77821517812500929, -34.26562499938548711, -102.3871387122750889 ) ) ;
#11931 = DIRECTION ( 'NONE',  ( -1.000000000000000000, -0.000000000000000000, -0.000000000000000000 ) ) ;
#11932 = AXIS2_PLACEMENT_3D ( 'NONE', #14252, #2338, #8209 ) ;
#11933 =( BOUNDED_CURVE ( )  B_SPLINE_CURVE ( 2, ( #7498, #16388, #3331, #7207, #16298, #2907, #7300, #13257, #8769 ),
 .UNSPECIFIED., .F., .F. ) 
 B_SPLINE_CURVE_WITH_KNOTS ( ( 3, 2, 2, 2, 3 ),
 ( 0.02083333333333332871, 0.02777777777777777624, 0.04166666666666666435, 0.05555555555555555247, 0.06250000000000002776 ),
 .UNSPECIFIED. ) 
 CURVE ( )  GEOMETRIC_REPRESENTATION_ITEM ( )  RATIONAL_B_SPLINE_CURVE ( ( 0.9330127018922191873, 0.9330127018922191873, 1.000000000000000000, 0.8660254037844387076, 1.000000000000000000, 0.8660254037844387076, 1.000000000000000000, 0.9330127018922190762, 0.9330127018922194093 ) ) 
 REPRESENTATION_ITEM ( '' )  );
#11934 = CARTESIAN_POINT ( 'NONE',  ( 235.5999999999999943, -34.70624999877096428, -48.26794919243124582 ) ) ;
#11935 = CARTESIAN_POINT ( 'NONE',  ( 232.5999999999999375, -29.99999999999999645, -47.00000000000010658 ) ) ;
#11936 = CARTESIAN_POINT ( 'NONE',  ( -85.15643035624999868, -31.45312499938548356, 101.5914258081833879 ) ) ;
#11937 = DIRECTION ( 'NONE',  ( -0.000000000000000000, -0.000000000000000000, 1.000000000000000000 ) ) ;
#11938 = CARTESIAN_POINT ( 'NONE',  ( 235.3564303562499447, -33.06562499938547717, -50.00000000000011369 ) ) ;
#11939 = ORIENTED_EDGE ( 'NONE', *, *, #13637, .T. ) ;
#11940 = ORIENTED_EDGE ( 'NONE', *, *, #13417, .F. ) ;
#11941 = CARTESIAN_POINT ( 'NONE',  ( -85.14613134194615895, -32.00000000000000000, 99.70214005991836359 ) ) ;
#11942 = CARTESIAN_POINT ( 'NONE',  ( -83.90000000000000568, -31.87500000000000000, 97.40192378864668399 ) ) ;
#11943 = CARTESIAN_POINT ( 'NONE',  ( -82.39999999999999147, -32.75624999877096855, 96.53589838486223584 ) ) ;
#11944 = CARTESIAN_POINT ( 'NONE',  ( 80.90000000000000568, -31.94999999999999929, 102.5980762113533018 ) ) ;
#11945 = CARTESIAN_POINT ( 'NONE',  ( -84.12306224665893239, -32.00000000000001421, -97.80849716182723341 ) ) ;
#11947 = CARTESIAN_POINT ( 'NONE',  ( 229.8435696437499871, -34.15312499938547575, 101.5914258081833879 ) ) ;
#11946 = AXIS2_PLACEMENT_3D ( 'NONE', #7733, #1969, #6374 ) ;
#11948 = CARTESIAN_POINT ( 'NONE',  ( 233.9782151781249411, -34.49062499938548143, -47.61286128772501769 ) ) ;
#11949 = CARTESIAN_POINT ( 'NONE',  ( 83.90000000000000568, -33.01874999877097139, -102.5980762113533018 ) ) ;
#11950 = CARTESIAN_POINT ( 'NONE',  ( 81.02178482187500208, -32.09062499938548285, -97.61286128772489690 ) ) ;
#11951 = EDGE_LOOP ( 'NONE', ( #10208, #4820 ) ) ;
#11952 = CARTESIAN_POINT ( 'NONE',  ( 234.0999999999999375, -30.29999999999999716, -47.40192378864679768 ) ) ;
#11953 = CARTESIAN_POINT ( 'NONE',  ( -82.39999999999999147, -31.40624999877096712, 96.99999999999998579 ) ) ;
#11954 = CARTESIAN_POINT ( 'NONE',  ( 82.39999999999999147, -34.30312499938548143, -96.81714838363319586 ) ) ;
#11955 = CYLINDRICAL_SURFACE ( 'NONE', #423, 5.199999999999996625 ) ;
#11956 = CARTESIAN_POINT ( 'NONE',  ( -82.39999999999999147, -33.20624999877097849, 97.00000000000000000 ) ) ;
#11957 = CARTESIAN_POINT ( 'NONE',  ( -85.40000000000000568, -34.91250000000000142, 101.7320508075688679 ) ) ;
#11958 = CARTESIAN_POINT ( 'NONE',  ( -82.39999999999999147, -30.78750000000000497, 103.4641016151377499 ) ) ;
#11959 = ORIENTED_EDGE ( 'NONE', *, *, #17770, .T. ) ;
#11960 = CARTESIAN_POINT ( 'NONE',  ( 82.40000000000000568, -33.43124999877096570, -102.9999999999999858 ) ) ;
#11961 = CARTESIAN_POINT ( 'NONE',  ( -82.40000000000000568, -31.18124999877096926, 102.9999999999999858 ) ) ;
#11962 = CARTESIAN_POINT ( 'NONE',  ( -79.39999999999999147, -32.47500000000000142, 99.99999999999998579 ) ) ;
#11963 = CARTESIAN_POINT ( 'NONE',  ( -79.39999999999999147, -33.33356250001228460, 98.26794919243110371 ) ) ;
#11964 = EDGE_CURVE ( 'NONE', #16006, #16850, #17309, .T. ) ;
#11965 =( BOUNDED_CURVE ( )  B_SPLINE_CURVE ( 2, ( #6531, #10915, #9252, #9445, #9348, #293, #480, #18255, #12477 ),
 .UNSPECIFIED., .F., .F. ) 
 B_SPLINE_CURVE_WITH_KNOTS ( ( 3, 2, 2, 2, 3 ),
 ( 0.7708333333333332593, 0.7777777777777777901, 0.7916666666666666297, 0.8055555555555555802, 0.8125000000000000000 ),
 .UNSPECIFIED. ) 
 CURVE ( )  GEOMETRIC_REPRESENTATION_ITEM ( )  RATIONAL_B_SPLINE_CURVE ( ( 0.9330127018922192983, 0.9330127018922187432, 1.000000000000000000, 0.8660254037844387076, 1.000000000000000000, 0.8660254037844387076, 1.000000000000000000, 0.9330127018922194093, 0.9330127018922194093 ) ) 
 REPRESENTATION_ITEM ( '' )  );
#11966 = EDGE_CURVE ( 'NONE', #12057, #14891, #1331, .T. ) ;
#11967 = LINE ( 'NONE', #8934, #14841 ) ;
#11968 = CARTESIAN_POINT ( 'NONE',  ( -80.90000000000000568, -32.04374999877096997, 102.5980762113533018 ) ) ;
#11969 = CARTESIAN_POINT ( 'NONE',  ( -79.64356964374999848, -31.26562499938548356, 99.99999999999998579 ) ) ;
#11970 = CARTESIAN_POINT ( 'NONE',  ( 85.16931825408417467, -32.00000000000000000, 99.76128878215590134 ) ) ;
#11971 = CARTESIAN_POINT ( 'NONE',  ( 83.77821517812500929, -33.02812499938548285, 102.3871387122750889 ) ) ;
#11972 = DIRECTION ( 'NONE',  ( 0.000000000000000000, -1.000000000000000000, 0.000000000000000000 ) ) ;
#11973 = CARTESIAN_POINT ( 'NONE',  ( -81.59615242270662350, -32.38259618943233420, -102.9999999999999716 ) ) ;
#11974 = CARTESIAN_POINT ( 'NONE',  ( 79.64356964375001269, -35.01562499938548711, -101.5914258081833879 ) ) ;
#11975 = CARTESIAN_POINT ( 'NONE',  ( -81.02178482187500208, -31.00312499938548783, -97.61286128772489690 ) ) ;
#11976 = VERTEX_POINT ( 'NONE', #16662 ) ;
#11977 = CARTESIAN_POINT ( 'NONE',  ( 85.15643035624999868, -30.66562499938548569, 98.40857419181659793 ) ) ;
#11978 = DIRECTION ( 'NONE',  ( 0.000000000000000000, 0.000000000000000000, -1.000000000000000000 ) ) ;
#11979 = CARTESIAN_POINT ( 'NONE',  ( 235.3564303562499447, -34.97812499938547859, -50.00000000000011369 ) ) ;
#11980 = EDGE_CURVE ( 'NONE', #2738, #16242, #3940, .T. ) ;
#11981 = CYLINDRICAL_SURFACE ( 'NONE', #14560, 3.000000000000002665 ) ;
#11982 = EDGE_CURVE ( 'NONE', #12892, #10996, #4698, .T. ) ;
#11983 = CARTESIAN_POINT ( 'NONE',  ( -82.39999999999999147, -31.26562499938549067, 96.81714838363319586 ) ) ;
#11984 = FACE_OUTER_BOUND ( 'NONE', #9579, .T. ) ;
#11985 = VERTEX_POINT ( 'NONE', #7574 ) ;
#11986 = EDGE_CURVE ( 'NONE', #15818, #11985, #6784, .T. ) ;
#11987 = CARTESIAN_POINT ( 'NONE',  ( -80.90000000000000568, -31.65000000000000568, -97.40192378864668399 ) ) ;
#11988 = DIRECTION ( 'NONE',  ( 1.000000000000000000, 0.000000000000000000, 0.000000000000000000 ) ) ;
#11989 = DIRECTION ( 'NONE',  ( -1.000000000000000000, 1.387778780781445478E-15, 2.407412430484046130E-31 ) ) ;
#11990 = CARTESIAN_POINT ( 'NONE',  ( -83.77821517812500929, -32.87812499938548427, -97.61286128772489690 ) ) ;
#11991 = CARTESIAN_POINT ( 'NONE',  ( -80.80006050676047380, -32.00000000000000000, -102.4537706361438438 ) ) ;
#11992 = CARTESIAN_POINT ( 'NONE',  ( 229.8435696437499871, -31.56562499938547717, 101.5914258081833879 ) ) ;
#11993 = CARTESIAN_POINT ( 'NONE',  ( -80.90000000000000568, -32.04768749875867684, 102.5980762113533018 ) ) ;
#11994 = CARTESIAN_POINT ( 'NONE',  ( -85.15643035625001289, -34.30312499938548854, 99.99999999999998579 ) ) ;
#11995 = CARTESIAN_POINT ( 'NONE',  ( -79.39999999999999147, -31.53749999999999787, 98.26794919243110371 ) ) ;
#11996 = CARTESIAN_POINT ( 'NONE',  ( 85.15643035625001289, -32.35312499938548569, 98.40857419181659793 ) ) ;
#11997 = CARTESIAN_POINT ( 'NONE',  ( -4.211140560182196957, -2.431303136016552013, -3.745885042887436178 ) ) ;
#11998 = FACE_OUTER_BOUND ( 'NONE', #4033, .T. ) ;
#11999 = CARTESIAN_POINT ( 'NONE',  ( 85.40000000000000568, -33.54374999877096286, -99.99999999999998579 ) ) ;
#12000 = CARTESIAN_POINT ( 'NONE',  ( 235.5999999999999943, -32.96249999999999858, 101.7320508075688537 ) ) ;
#12001 = ORIENTED_EDGE ( 'NONE', *, *, #17238, .F. ) ;
#12002 = CARTESIAN_POINT ( 'NONE',  ( 233.9782151781249411, -34.45312499938548001, -52.38713871227520968 ) ) ;
#12003 =( NAMED_UNIT ( * ) PLANE_ANGLE_UNIT ( ) SI_UNIT ( $, .RADIAN. ) );
#12004 = CARTESIAN_POINT ( 'NONE',  ( 234.0999999999999375, -35.19374999877096855, 102.5980762113533018 ) ) ;
#12005 = CARTESIAN_POINT ( 'NONE',  ( 231.0999999999999375, -33.46874999877096002, -47.40192378864679768 ) ) ;
#12006 = CARTESIAN_POINT ( 'NONE',  ( -81.02178482187500208, -32.69062499938548427, 102.3871387122750889 ) ) ;
#12007 = VERTEX_POINT ( 'NONE', #17145 ) ;
#12008 = ORIENTED_EDGE ( 'NONE', *, *, #18216, .F. ) ;
#12009 = CARTESIAN_POINT ( 'NONE',  ( 105.1999999999999744, -34.99999999999999289, -100.0000000000000000 ) ) ;
#12010 = DIRECTION ( 'NONE',  ( 0.000000000000000000, 0.000000000000000000, -1.000000000000000000 ) ) ;
#12011 = CARTESIAN_POINT ( 'NONE',  ( -85.40000000000000568, -33.56250000000000000, -98.26794919243111792 ) ) ;
#12012 = VERTEX_POINT ( 'NONE', #3369 ) ;
#12013 = DIRECTION ( 'NONE',  ( 0.000000000000000000, -1.000000000000000000, 0.000000000000000000 ) ) ;
#12014 = AXIS2_PLACEMENT_3D ( 'NONE', #9882, #11147, #18777 ) ;
#12015 = CARTESIAN_POINT ( 'NONE',  ( -85.15643035624999868, -34.34062499938548285, 98.40857419181659793 ) ) ;
#12016 = CARTESIAN_POINT ( 'NONE',  ( -80.90000000000000568, -33.89999999999999858, 102.5980762113533018 ) ) ;
#12017 =( BOUNDED_CURVE ( )  B_SPLINE_CURVE ( 2, ( #12133, #1771, #18002, #10285, #16338, #2947, #8901, #13690, #14966 ),
 .UNSPECIFIED., .F., .F. ) 
 B_SPLINE_CURVE_WITH_KNOTS ( ( 3, 2, 2, 2, 3 ),
 ( 0.7291666666666665186, 0.7361111111111111605, 0.7500000000000000000, 0.7638888888888888395, 0.7708333333333332593 ),
 .UNSPECIFIED. ) 
 CURVE ( )  GEOMETRIC_REPRESENTATION_ITEM ( )  RATIONAL_B_SPLINE_CURVE ( ( 0.9330127018922194093, 0.9330127018922177440, 1.000000000000000000, 0.8660254037844387076, 1.000000000000000000, 0.8660254037844387076, 1.000000000000000000, 0.9330127018922198534, 0.9330127018922192983 ) ) 
 REPRESENTATION_ITEM ( '' )  );
#12018 = CARTESIAN_POINT ( 'NONE',  ( -83.90000000000000568, -30.76874999877097139, 102.5980762113533018 ) ) ;
#12019 = CARTESIAN_POINT ( 'NONE',  ( 111.5000000000000142, 12.69999999999998508, 110.0000000000000142 ) ) ;
#12020 = EDGE_CURVE ( 'NONE', #10773, #15647, #13598, .T. ) ;
#12021 = SURFACE_SIDE_STYLE ('',( #7818 ) ) ;
#12022 = LINE ( 'NONE', #4807, #16498 ) ;
#12023 = LINE ( 'NONE', #7437, #4939 ) ;
#12024 = CARTESIAN_POINT ( 'NONE',  ( 232.5999999999999375, -30.47812499938547859, 103.1828516163667899 ) ) ;
#12025 = ORIENTED_EDGE ( 'NONE', *, *, #17619, .T. ) ;
#12026 =( NAMED_UNIT ( * ) PLANE_ANGLE_UNIT ( ) SI_UNIT ( $, .RADIAN. ) );
#12027 = CARTESIAN_POINT ( 'NONE',  ( -83.77821517812500929, -32.31562499938548427, -97.61286128772489690 ) ) ;
#12028 = CARTESIAN_POINT ( 'NONE',  ( 3.472371940585993855, 2.614027278893175321, -3.320322319201766792 ) ) ;
#12029 = AXIS2_PLACEMENT_3D ( 'NONE', #13009, #18978, #5602 ) ;
#12030 = CARTESIAN_POINT ( 'NONE',  ( 2.000000000000008882, 3.464101615137749945, 0.000000000000000000 ) ) ;
#12031 = CARTESIAN_POINT ( 'NONE',  ( 69.99999999999998579, -34.99999999999999289, 150.0000000000000000 ) ) ;
#12032 = CARTESIAN_POINT ( 'NONE',  ( -79.64356964374999848, -31.26562499938548356, 99.99999999999998579 ) ) ;
#12033 = CARTESIAN_POINT ( 'NONE',  ( 82.39999999999999147, -33.48750000000000426, 97.00000000000000000 ) ) ;
#12034 = CARTESIAN_POINT ( 'NONE',  ( 232.5999999999999375, -32.50312499938547717, -53.18285161636690361 ) ) ;
#12035 = ORIENTED_EDGE ( 'NONE', *, *, #161, .F. ) ;
#12036 = ORIENTED_EDGE ( 'NONE', *, *, #1235, .F. ) ;
#12037 = CARTESIAN_POINT ( 'NONE',  ( -83.20384757729335945, -31.89240381056766793, 96.99999999999997158 ) ) ;
#12038 = CARTESIAN_POINT ( 'NONE',  ( -79.39999999999999147, -30.71250000000000568, 101.7320508075688537 ) ) ;
#12039 = CARTESIAN_POINT ( 'NONE',  ( -80.90000000000000568, -32.34374999877096712, 97.40192378864668399 ) ) ;
#12040 = CARTESIAN_POINT ( 'NONE',  ( 85.40000000000000568, -31.38749999999999574, 101.7320508075688679 ) ) ;
#12041 = CARTESIAN_POINT ( 'NONE',  ( 111.0000000000000000, 10.19999999999997620, -137.3499999999999943 ) ) ;
#12042 = CARTESIAN_POINT ( 'NONE',  ( 229.8435696437499871, -33.25312499938547717, 101.5914258081833879 ) ) ;
#12043 = VECTOR ( 'NONE', #17509, 1000.000000000000000 ) ;
#12044 = CARTESIAN_POINT ( 'NONE',  ( 83.90000000000000568, -32.26874999877097139, 102.5980762113533018 ) ) ;
#12045 = CARTESIAN_POINT ( 'NONE',  ( 80.24181665639378025, -32.00000000000000000, -97.97695283462226712 ) ) ;
#12046 =( BOUNDED_SURFACE ( )  B_SPLINE_SURFACE ( 1, 2, ( 
 ( #8365, #15795, #3965, #15700, #12764, #2687, #9831, #6999, #13050, #11584, #10123, #18733, #11491, #17165, #8454, #854, #14604, #5253, #11199, #3770, #9737, #2303, #14317, #8268, #9932, #15890, #6910, #956, #12859, #18830, #5452, #2496, #11393, #17355, #5544, #17455, #16369, #10316, #3074, #63, #10405, #14797, #5730, #11868, #16467, #4353, #4546, #13235, #2792, #10501, #16273, #1619, #17750, #3168, #11679, #17934, #19311, #4449, #9034, #19209, #16565, #14998, #7570, #8743, #13524, #11773, #1424, #160, #2977, #14696, #7281, #2885, #8841, #6113, #12063, #14896, #1526, #8933, #7476, #7377, #13334, #9128, #18038, #15090, #13433, #5923, #4651, #10600, #5824, #6017, #1707, #11963, #4258, #16182, #17836, #7660, #19110, #17645, #10217, #1334, #6869, #13616, #18590, #11251, #625, #16659, #3632, #17022, #910, #2071, #12617, #9493, #14273, #8230, #10692, #5112, #8028, #6772, #15850, #3261, #9888, #17215, #5206, #6573, #11053, #12816, #12720, #12521, #15461, #2261, #13987, #2459, #17314, #18492, #6215, #259, #9595 ),
 ( #11349, #3820, #9789, #15559, #15751, #2173, #8130, #2357, #11153, #14082, #720, #6676, #17122, #5309, #8319, #9693, #15655, #3728, #14178, #813, #12162, #18692, #18781, #5406, #3921, #18129, #4746, #5599, #14553, #19164, #11544, #2638, #5688, #17412, #4212, #5777, #8705, #8603, #9986, #5879, #16236, #14655, #17506, #14457, #18976, #1089, #7047, #16327, #7238, #10079, #4117, #2841, #16037, #11729, #15941, #8798, #19261, #14367, #2543, #1193, #17599, #13005, #13193, #10275, #13099, #18879, #8505, #10171, #7148, #19069, #8415, #4406, #17697, #4312, #1386, #16134, #10363, #11637, #1004, #6959, #2744, #11829, #14753, #17796, #1290, #7333, #13286, #12911, #5501, #11448, #4025, #16614, #7431, #22, #9080, #10646, #9272, #4697, #17989, #15142, #15241, #2936, #7621, #314, #8990, #5972, #12016, #6070, #1855, #10456, #1669, #17893, #3315, #3220, #11922, #13481, #16420, #1758, #4893, #4501, #18276, #6265, #13573, #14952, #121, #7813, #7716, #1577, #3030, #9178, #7525, #10837, #6357, #4600, #14849, #8889, #10559 ),
 ( #212, #12118, #16520, #13676, #12210, #18180, #3123, #18089, #15046, #4803, #1474, #12309, #10742, #13388, #6168, #16707, #13769, #409, #6649, #13960, #15533, #5282, #6551, #18376, #5378, #3510, #12496, #602, #15331, #500, #11227, #2150, #10937, #18562, #3417, #884, #5178, #788, #11029, #12594, #12790, #14154, #8107, #8296, #7907, #9765, #14246, #9470, #6845, #13858, #11124, #18759, #17192, #17092, #18663, #16808, #3705, #18467, #14060, #3796, #5087, #4994, #9369, #15432, #16993, #3605, #1949, #6453, #15726, #694, #16904, #9671, #12405, #2045, #15632, #6743, #9566, #2237, #8004, #12690, #8203, #2332, #2432, #4285, #2818, #3997, #8775, #8391, #1164, #1361, #5754, #11608, #7123, #11423, #17383, #19236, #7305, #8677, #14630, #10250, #19042, #13262, #11521, #11326, #9862, #12980, #14725, #7212, #17291, #13076, #17482, #13165, #3894, #9962, #5665, #15822, #17577, #14342, #980, #4091, #4188, #17672, #10148, #7026, #16110, #16212, #6935, #16012, #1265, #15916, #12886, #1069, #14435, #18857, #5477, #10053, #2521 ),
 ( #8478, #8577, #18950, #19137, #2717, #2616, #5574, #14532, #11703, #3193, #10430, #10623, #19321, #8865, #16589, #16394, #7689, #4477, #9247, #11806, #4674, #6046, #10528, #9152, #5948, #3288, #15115, #1731, #14822, #13645, #17866, #1554, #286, #16496, #1450, #13366, #3004, #8960, #6237, #12185, #1828, #18153, #4775, #10718, #13549, #7788, #11993, #13742, #4382, #7502, #15211, #16682, #5852, #15023, #17961, #17775, #10339, #11895, #189, #16303, #6139, #2913, #7403, #4571, #12089, #14928, #7596, #13458, #18063, #93, #3098, #9058, #1643, #6424, #3392, #9440, #3480, #6715, #7882, #18440, #15306, #762, #14033, #16777, #10910, #13833, #12567, #2305, #9343, #15703, #3681, #5059, #12380, #16876, #12661, #18535, #18346, #1919, #8080, #475, #8269, #3771, #4968, #12285, #6333, #15406, #5255, #2016, #8177, #15505, #11001, #9539, #7976, #2120, #9646, #11097, #13932, #669, #571, #15607, #18249, #9738, #4867, #6526, #18634, #12472, #6618, #3579, #5151, #16968, #380, #17066, #2213, #14124, #11201, #17167, #10811 ) ),
 .UNSPECIFIED., .F., .F., .F. ) 
 B_SPLINE_SURFACE_WITH_KNOTS ( ( 2, 1, 1, 2 ),
 ( 3, 2, 2, 2, 2, 2, 2, 2, 2, 2, 2, 2, 2, 2, 2, 2, 2, 2, 2, 2, 2, 2, 2, 2, 2, 2, 2, 2, 2, 2, 2, 2, 2, 2, 2, 2, 2, 2, 2, 2, 2, 2, 2, 2, 2, 2, 2, 2, 2, 2, 2, 2, 2, 2, 2, 2, 2, 2, 2, 2, 2, 2, 2, 2, 2, 2, 2, 2, 3 ),
 ( -0.01000000000000000021, 0.000000000000000000, 1.000000000000000000, 1.010000000000000009 ),
 ( -0.009258785004222062215, 0.000000000000000000, 0.01388888888888888812, 0.02777777777777777624, 0.04166666666666666435, 0.05555555555555555247, 0.06944444444444444753, 0.08333333333333332871, 0.09722222222222222376, 0.1111111111111111049, 0.1250000000000000000, 0.1388888888888888951, 0.1527777777777777901, 0.1666666666666666574, 0.1805555555555555525, 0.1944444444444444475, 0.2083333333333333426, 0.2222222222222222099, 0.2361111111111111049, 0.2500000000000000000, 0.2638888888888888951, 0.2777777777777777901, 0.2916666666666666852, 0.3055555555555555802, 0.3194444444444444198, 0.3333333333333333148, 0.3472222222222222099, 0.3611111111111111049, 0.3750000000000000000, 0.3888888888888888951, 0.4027777777777777901, 0.4166666666666666852, 0.4305555555555555802, 0.4444444444444444198, 0.4583333333333333148, 0.4722222222222222099, 0.4861111111111111049, 0.5000000000000000000, 0.5138888888888888395, 0.5277777777777777901, 0.5416666666666666297, 0.5555555555555555802, 0.5694444444444444198, 0.5833333333333333703, 0.5972222222222222099, 0.6111111111111111605, 0.6250000000000000000, 0.6388888888888888395, 0.6527777777777777901, 0.6666666666666666297, 0.6805555555555555802, 0.6944444444444444198, 0.7083333333333333703, 0.7222222222222222099, 0.7361111111111111605, 0.7500000000000000000, 0.7638888888888888395, 0.7777777777777777901, 0.7916666666666666297, 0.8055555555555555802, 0.8194444444444444198, 0.8333333333333333703, 0.8472222222222222099, 0.8611111111111111605, 0.8750000000000000000, 0.8888888888888888395, 0.9027777777777777901, 0.9166666666666666297, 0.9258785004222062076 ),
 .UNSPECIFIED. ) 
 GEOMETRIC_REPRESENTATION_ITEM ( )  RATIONAL_B_SPLINE_SURFACE ( (
 ( 1.000000000000000000, 1.000000000000000000, 1.000000000000000000, 0.8660254037844387076, 1.000000000000000000, 0.8660254037844387076, 1.000000000000000000, 0.8660254037844387076, 1.000000000000000000, 0.8660254037844387076, 1.000000000000000000, 0.8660254037844387076, 1.000000000000000000, 0.8660254037844387076, 1.000000000000000000, 0.8660254037844387076, 1.000000000000000000, 0.8660254037844387076, 1.000000000000000000, 0.8660254037844387076, 1.000000000000000000, 0.8660254037844387076, 1.000000000000000000, 0.8660254037844387076, 1.000000000000000000, 0.8660254037844387076, 1.000000000000000000, 0.8660254037844387076, 1.000000000000000000, 0.8660254037844387076, 1.000000000000000000, 0.8660254037844387076, 1.000000000000000000, 0.8660254037844387076, 1.000000000000000000, 0.8660254037844387076, 1.000000000000000000, 0.8660254037844387076, 1.000000000000000000, 0.8660254037844387076, 1.000000000000000000, 0.8660254037844387076, 1.000000000000000000, 0.8660254037844387076, 1.000000000000000000, 0.8660254037844387076, 1.000000000000000000, 0.8660254037844387076, 1.000000000000000000, 0.8660254037844387076, 1.000000000000000000, 0.8660254037844387076, 1.000000000000000000, 0.8660254037844387076, 1.000000000000000000, 0.8660254037844387076, 1.000000000000000000, 0.8660254037844387076, 1.000000000000000000, 0.8660254037844387076, 1.000000000000000000, 0.8660254037844387076, 1.000000000000000000, 0.8660254037844387076, 1.000000000000000000, 0.8660254037844387076, 1.000000000000000000, 0.8660254037844387076, 1.000000000000000000, 0.8660254037844387076, 1.000000000000000000, 0.8660254037844387076, 1.000000000000000000, 0.8660254037844387076, 1.000000000000000000, 0.8660254037844387076, 1.000000000000000000, 0.8660254037844387076, 1.000000000000000000, 0.8660254037844387076, 1.000000000000000000, 0.8660254037844387076, 1.000000000000000000, 0.8660254037844387076, 1.000000000000000000, 0.8660254037844387076, 1.000000000000000000, 0.8660254037844387076, 1.000000000000000000, 0.8660254037844387076, 1.000000000000000000, 0.8660254037844387076, 1.000000000000000000, 0.8660254037844387076, 1.000000000000000000, 0.8660254037844387076, 1.000000000000000000, 0.8660254037844387076, 1.000000000000000000, 0.8660254037844387076, 1.000000000000000000, 0.8660254037844387076, 1.000000000000000000, 0.8660254037844387076, 1.000000000000000000, 0.8660254037844387076, 1.000000000000000000, 0.8660254037844387076, 1.000000000000000000, 0.8660254037844387076, 1.000000000000000000, 0.8660254037844387076, 1.000000000000000000, 0.8660254037844387076, 1.000000000000000000, 0.8660254037844387076, 1.000000000000000000, 0.8660254037844387076, 1.000000000000000000, 0.8660254037844387076, 1.000000000000000000, 0.8660254037844387076, 1.000000000000000000, 0.8660254037844387076, 1.000000000000000000, 0.8660254037844387076, 1.000000000000000000, 0.8660254037844387076, 1.000000000000000000, 0.8660254037844387076, 1.000000000000000000, 0.8660254037844387076, 1.000000000000000000, 0.8660254037844387076, 1.000000000000000000, 0.9111410770381633828, 0.9401538762233125901),
 ( 1.000000000000000000, 1.000000000000000000, 1.000000000000000000, 0.8660254037844387076, 1.000000000000000000, 0.8660254037844387076, 1.000000000000000000, 0.8660254037844387076, 1.000000000000000000, 0.8660254037844387076, 1.000000000000000000, 0.8660254037844387076, 1.000000000000000000, 0.8660254037844387076, 1.000000000000000000, 0.8660254037844387076, 1.000000000000000000, 0.8660254037844387076, 1.000000000000000000, 0.8660254037844387076, 1.000000000000000000, 0.8660254037844387076, 1.000000000000000000, 0.8660254037844387076, 1.000000000000000000, 0.8660254037844387076, 1.000000000000000000, 0.8660254037844387076, 1.000000000000000000, 0.8660254037844387076, 1.000000000000000000, 0.8660254037844387076, 1.000000000000000000, 0.8660254037844387076, 1.000000000000000000, 0.8660254037844387076, 1.000000000000000000, 0.8660254037844387076, 1.000000000000000000, 0.8660254037844387076, 1.000000000000000000, 0.8660254037844387076, 1.000000000000000000, 0.8660254037844387076, 1.000000000000000000, 0.8660254037844387076, 1.000000000000000000, 0.8660254037844387076, 1.000000000000000000, 0.8660254037844387076, 1.000000000000000000, 0.8660254037844387076, 1.000000000000000000, 0.8660254037844387076, 1.000000000000000000, 0.8660254037844387076, 1.000000000000000000, 0.8660254037844387076, 1.000000000000000000, 0.8660254037844387076, 1.000000000000000000, 0.8660254037844387076, 1.000000000000000000, 0.8660254037844387076, 1.000000000000000000, 0.8660254037844387076, 1.000000000000000000, 0.8660254037844387076, 1.000000000000000000, 0.8660254037844387076, 1.000000000000000000, 0.8660254037844387076, 1.000000000000000000, 0.8660254037844387076, 1.000000000000000000, 0.8660254037844387076, 1.000000000000000000, 0.8660254037844387076, 1.000000000000000000, 0.8660254037844387076, 1.000000000000000000, 0.8660254037844387076, 1.000000000000000000, 0.8660254037844387076, 1.000000000000000000, 0.8660254037844387076, 1.000000000000000000, 0.8660254037844387076, 1.000000000000000000, 0.8660254037844387076, 1.000000000000000000, 0.8660254037844387076, 1.000000000000000000, 0.8660254037844387076, 1.000000000000000000, 0.8660254037844387076, 1.000000000000000000, 0.8660254037844387076, 1.000000000000000000, 0.8660254037844387076, 1.000000000000000000, 0.8660254037844387076, 1.000000000000000000, 0.8660254037844387076, 1.000000000000000000, 0.8660254037844387076, 1.000000000000000000, 0.8660254037844387076, 1.000000000000000000, 0.8660254037844387076, 1.000000000000000000, 0.8660254037844387076, 1.000000000000000000, 0.8660254037844387076, 1.000000000000000000, 0.8660254037844387076, 1.000000000000000000, 0.8660254037844387076, 1.000000000000000000, 0.8660254037844387076, 1.000000000000000000, 0.8660254037844387076, 1.000000000000000000, 0.8660254037844387076, 1.000000000000000000, 0.8660254037844387076, 1.000000000000000000, 0.8660254037844387076, 1.000000000000000000, 0.8660254037844387076, 1.000000000000000000, 0.8660254037844387076, 1.000000000000000000, 0.8660254037844387076, 1.000000000000000000, 0.9111410770381633828, 0.9401538762233125901),
 ( 1.000000000000000000, 1.000000000000000000, 1.000000000000000000, 0.8660254037844387076, 1.000000000000000000, 0.8660254037844387076, 1.000000000000000000, 0.8660254037844387076, 1.000000000000000000, 0.8660254037844387076, 1.000000000000000000, 0.8660254037844387076, 1.000000000000000000, 0.8660254037844387076, 1.000000000000000000, 0.8660254037844387076, 1.000000000000000000, 0.8660254037844387076, 1.000000000000000000, 0.8660254037844387076, 1.000000000000000000, 0.8660254037844387076, 1.000000000000000000, 0.8660254037844387076, 1.000000000000000000, 0.8660254037844387076, 1.000000000000000000, 0.8660254037844387076, 1.000000000000000000, 0.8660254037844387076, 1.000000000000000000, 0.8660254037844387076, 1.000000000000000000, 0.8660254037844387076, 1.000000000000000000, 0.8660254037844387076, 1.000000000000000000, 0.8660254037844387076, 1.000000000000000000, 0.8660254037844387076, 1.000000000000000000, 0.8660254037844387076, 1.000000000000000000, 0.8660254037844387076, 1.000000000000000000, 0.8660254037844387076, 1.000000000000000000, 0.8660254037844387076, 1.000000000000000000, 0.8660254037844387076, 1.000000000000000000, 0.8660254037844387076, 1.000000000000000000, 0.8660254037844387076, 1.000000000000000000, 0.8660254037844387076, 1.000000000000000000, 0.8660254037844387076, 1.000000000000000000, 0.8660254037844387076, 1.000000000000000000, 0.8660254037844387076, 1.000000000000000000, 0.8660254037844387076, 1.000000000000000000, 0.8660254037844387076, 1.000000000000000000, 0.8660254037844387076, 1.000000000000000000, 0.8660254037844387076, 1.000000000000000000, 0.8660254037844387076, 1.000000000000000000, 0.8660254037844387076, 1.000000000000000000, 0.8660254037844387076, 1.000000000000000000, 0.8660254037844387076, 1.000000000000000000, 0.8660254037844387076, 1.000000000000000000, 0.8660254037844387076, 1.000000000000000000, 0.8660254037844387076, 1.000000000000000000, 0.8660254037844387076, 1.000000000000000000, 0.8660254037844387076, 1.000000000000000000, 0.8660254037844387076, 1.000000000000000000, 0.8660254037844387076, 1.000000000000000000, 0.8660254037844387076, 1.000000000000000000, 0.8660254037844387076, 1.000000000000000000, 0.8660254037844387076, 1.000000000000000000, 0.8660254037844387076, 1.000000000000000000, 0.8660254037844387076, 1.000000000000000000, 0.8660254037844387076, 1.000000000000000000, 0.8660254037844387076, 1.000000000000000000, 0.8660254037844387076, 1.000000000000000000, 0.8660254037844387076, 1.000000000000000000, 0.8660254037844387076, 1.000000000000000000, 0.8660254037844387076, 1.000000000000000000, 0.8660254037844387076, 1.000000000000000000, 0.8660254037844387076, 1.000000000000000000, 0.8660254037844387076, 1.000000000000000000, 0.8660254037844387076, 1.000000000000000000, 0.8660254037844387076, 1.000000000000000000, 0.8660254037844387076, 1.000000000000000000, 0.8660254037844387076, 1.000000000000000000, 0.8660254037844387076, 1.000000000000000000, 0.8660254037844387076, 1.000000000000000000, 0.8660254037844387076, 1.000000000000000000, 0.9111410770381633828, 0.9401538762233125901),
 ( 1.000000000000000000, 1.000000000000000000, 1.000000000000000000, 0.8660254037844387076, 1.000000000000000000, 0.8660254037844387076, 1.000000000000000000, 0.8660254037844387076, 1.000000000000000000, 0.8660254037844387076, 1.000000000000000000, 0.8660254037844387076, 1.000000000000000000, 0.8660254037844387076, 1.000000000000000000, 0.8660254037844387076, 1.000000000000000000, 0.8660254037844387076, 1.000000000000000000, 0.8660254037844387076, 1.000000000000000000, 0.8660254037844387076, 1.000000000000000000, 0.8660254037844387076, 1.000000000000000000, 0.8660254037844387076, 1.000000000000000000, 0.8660254037844387076, 1.000000000000000000, 0.8660254037844387076, 1.000000000000000000, 0.8660254037844387076, 1.000000000000000000, 0.8660254037844387076, 1.000000000000000000, 0.8660254037844387076, 1.000000000000000000, 0.8660254037844387076, 1.000000000000000000, 0.8660254037844387076, 1.000000000000000000, 0.8660254037844387076, 1.000000000000000000, 0.8660254037844387076, 1.000000000000000000, 0.8660254037844387076, 1.000000000000000000, 0.8660254037844387076, 1.000000000000000000, 0.8660254037844387076, 1.000000000000000000, 0.8660254037844387076, 1.000000000000000000, 0.8660254037844387076, 1.000000000000000000, 0.8660254037844387076, 1.000000000000000000, 0.8660254037844387076, 1.000000000000000000, 0.8660254037844387076, 1.000000000000000000, 0.8660254037844387076, 1.000000000000000000, 0.8660254037844387076, 1.000000000000000000, 0.8660254037844387076, 1.000000000000000000, 0.8660254037844387076, 1.000000000000000000, 0.8660254037844387076, 1.000000000000000000, 0.8660254037844387076, 1.000000000000000000, 0.8660254037844387076, 1.000000000000000000, 0.8660254037844387076, 1.000000000000000000, 0.8660254037844387076, 1.000000000000000000, 0.8660254037844387076, 1.000000000000000000, 0.8660254037844387076, 1.000000000000000000, 0.8660254037844387076, 1.000000000000000000, 0.8660254037844387076, 1.000000000000000000, 0.8660254037844387076, 1.000000000000000000, 0.8660254037844387076, 1.000000000000000000, 0.8660254037844387076, 1.000000000000000000, 0.8660254037844387076, 1.000000000000000000, 0.8660254037844387076, 1.000000000000000000, 0.8660254037844387076, 1.000000000000000000, 0.8660254037844387076, 1.000000000000000000, 0.8660254037844387076, 1.000000000000000000, 0.8660254037844387076, 1.000000000000000000, 0.8660254037844387076, 1.000000000000000000, 0.8660254037844387076, 1.000000000000000000, 0.8660254037844387076, 1.000000000000000000, 0.8660254037844387076, 1.000000000000000000, 0.8660254037844387076, 1.000000000000000000, 0.8660254037844387076, 1.000000000000000000, 0.8660254037844387076, 1.000000000000000000, 0.8660254037844387076, 1.000000000000000000, 0.8660254037844387076, 1.000000000000000000, 0.8660254037844387076, 1.000000000000000000, 0.8660254037844387076, 1.000000000000000000, 0.8660254037844387076, 1.000000000000000000, 0.8660254037844387076, 1.000000000000000000, 0.8660254037844387076, 1.000000000000000000, 0.8660254037844387076, 1.000000000000000000, 0.9111410770381633828, 0.9401538762233125901) ) ) 
 REPRESENTATION_ITEM ( '' )  SURFACE ( )  );
#12047 = CARTESIAN_POINT ( 'NONE',  ( 82.39999999999999147, -31.82812499938548356, -103.1828516163667899 ) ) ;
#12048 = EDGE_LOOP ( 'NONE', ( #5327, #16142, #556, #8237 ) ) ;
#12049 = CARTESIAN_POINT ( 'NONE',  ( 232.5999999999999375, -32.58749999999999858, -46.53589838486234953 ) ) ;
#12050 = DIRECTION ( 'NONE',  ( 0.000000000000000000, 1.000000000000000000, 0.000000000000000000 ) ) ;
#12051 = CARTESIAN_POINT ( 'NONE',  ( 79.64356964374999848, -34.41562499938548569, -99.99999999999998579 ) ) ;
#12052 =( GEOMETRIC_REPRESENTATION_CONTEXT ( 3 ) GLOBAL_UNCERTAINTY_ASSIGNED_CONTEXT ( ( #615 ) ) GLOBAL_UNIT_ASSIGNED_CONTEXT ( ( #15735, #17004, #9774 ) ) REPRESENTATION_CONTEXT ( 'NONE', 'WORKASPACE' ) );
#12053 = FACE_OUTER_BOUND ( 'NONE', #1464, .T. ) ;
#12054 = CARTESIAN_POINT ( 'NONE',  ( 229.8435696437499303, -31.15312499938548285, -50.00000000000011369 ) ) ;
#12055 = AXIS2_PLACEMENT_3D ( 'NONE', #10621, #14627, #1262 ) ;
#12056 = CARTESIAN_POINT ( 'NONE',  ( -79.39999999999999147, -31.57499999999999929, 99.99999999999998579 ) ) ;
#12057 = VERTEX_POINT ( 'NONE', #15585 ) ;
#12058 = CARTESIAN_POINT ( 'NONE',  ( -85.39923668279692492, -34.99824194014708922, 99.66573144631155401 ) ) ;
#12059 = EDGE_CURVE ( 'NONE', #15031, #12702, #6697, .T. ) ;
#12060 = B_SPLINE_CURVE_WITH_KNOTS ( 'NONE', 3,
 ( #12525, #12726, #10962, #9498, #18496 ),
 .UNSPECIFIED., .F., .F.,
 ( 4, 1, 4 ),
 ( 0.000000000000000000, 0.002020725942163690940, 0.004041451884327381880 ),
 .UNSPECIFIED. ) ;
#12061 = CYLINDRICAL_SURFACE ( 'NONE', #1014, 3.000000000000009770 ) ;
#12062 = CARTESIAN_POINT ( 'NONE',  ( 85.15643035625001289, -30.14062499938548711, 99.99999999999998579 ) ) ;
#12063 = CARTESIAN_POINT ( 'NONE',  ( -85.40000000000000568, -32.69606250001229597, 99.99999999999998579 ) ) ;
#12064 = B_SPLINE_CURVE_WITH_KNOTS ( 'NONE', 3,
 ( #758, #6522, #566, #2301, #3867, #8267, #14215, #18435 ),
 .UNSPECIFIED., .F., .F.,
 ( 4, 2, 2, 4 ),
 ( 0.000000000000000000, 0.002450665683189819262, 0.003675998524784728893, 0.004901331366379639391 ),
 .UNSPECIFIED. ) ;
#12065 = DIRECTION ( 'NONE',  ( 9.251858538542962756E-15, 0.000000000000000000, -1.000000000000000000 ) ) ;
#12066 = CARTESIAN_POINT ( 'NONE',  ( -83.90000000000000568, -32.32500000000000284, 97.40192378864668399 ) ) ;
#12067 = AXIS2_PLACEMENT_3D ( 'NONE', #16061, #9084, #11663 ) ;
#12068 = CARTESIAN_POINT ( 'NONE',  ( 84.74067385206578251, -31.99999999999998579, 101.4666071953140829 ) ) ;
#12069 = CARTESIAN_POINT ( 'NONE',  ( 85.15643035624999868, -30.55312499938548854, 98.40857419181659793 ) ) ;
#12070 = CARTESIAN_POINT ( 'NONE',  ( -82.40000000000001990, -32.08124999877097139, 103.0000000000000000 ) ) ;
#12071 = DIRECTION ( 'NONE',  ( 1.000000000000000000, 0.000000000000000000, 0.000000000000000000 ) ) ;
#12072 = CARTESIAN_POINT ( 'NONE',  ( 85.15643035624999868, -35.16562499938547859, -101.5914258081833879 ) ) ;
#12073 = CARTESIAN_POINT ( 'NONE',  ( 0.000000000000000000, 0.000000000000000000, -4.484454397937119197 ) ) ;
#12074 = VERTEX_POINT ( 'NONE', #14105 ) ;
#12075 = CARTESIAN_POINT ( 'NONE',  ( 83.77821517812500929, -31.22812499938548569, 102.3871387122750889 ) ) ;
#12076 = CARTESIAN_POINT ( 'NONE',  ( 244.7999999999999545, -4.999999999999976907, 153.0000000000000000 ) ) ;
#12077 = SURFACE_STYLE_USAGE ( .BOTH. , #177 ) ;
#12078 = CARTESIAN_POINT ( 'NONE',  ( -83.77821517812500929, -30.62812499938548783, 102.3871387122750889 ) ) ;
#12079 = CARTESIAN_POINT ( 'NONE',  ( 80.90000000000000568, -33.84374999877096712, -102.5980762113533018 ) ) ;
#12080 = VERTEX_POINT ( 'NONE', #16949 ) ;
#12081 = CARTESIAN_POINT ( 'NONE',  ( -85.40000000000000568, -30.45000000000000284, -99.99999999999998579 ) ) ;
#12082 = AXIS2_PLACEMENT_3D ( 'NONE', #13012, #918, #11550 ) ;
#12083 =( BOUNDED_CURVE ( )  B_SPLINE_CURVE ( 2, ( #5462, #16091, #11404, #17366, #2697, #1054, #14511, #7105, #13061 ),
 .UNSPECIFIED., .F., .F. ) 
 B_SPLINE_CURVE_WITH_KNOTS ( ( 3, 2, 2, 2, 3 ),
 ( 0.7291666666666667407, 0.7361111111111111605, 0.7500000000000000000, 0.7638888888888888395, 0.7708333333333332593 ),
 .UNSPECIFIED. ) 
 CURVE ( )  GEOMETRIC_REPRESENTATION_ITEM ( )  RATIONAL_B_SPLINE_CURVE ( ( 0.9330127018922192983, 0.9330127018922198534, 1.000000000000000000, 0.8660254037844387076, 1.000000000000000000, 0.8660254037844387076, 1.000000000000000000, 0.9330127018922198534, 0.9330127018922192983 ) ) 
 REPRESENTATION_ITEM ( '' )  );
#12084 = CARTESIAN_POINT ( 'NONE',  ( 85.40000000000000568, -34.05000000000000426, -99.99999999999998579 ) ) ;
#12085 = CARTESIAN_POINT ( 'NONE',  ( 85.40000000000000568, -34.93124999877096570, -98.26794919243111792 ) ) ;
#12086 = CARTESIAN_POINT ( 'NONE',  ( -85.15643035624999868, -32.46562499938548996, -98.40857419181659793 ) ) ;
#12087 = CARTESIAN_POINT ( 'NONE',  ( 232.5999999999999375, -33.65624999877096002, -53.00000000000011369 ) ) ;
#12088 = CARTESIAN_POINT ( 'NONE',  ( 235.3564303562499447, -30.92812499938547788, 99.99999999999998579 ) ) ;
#12089 = CARTESIAN_POINT ( 'NONE',  ( -83.90000000000000568, -32.72268749875867400, 97.40192378864668399 ) ) ;
#12090 = AXIS2_PLACEMENT_3D ( 'NONE', #13685, #6276, #3616 ) ;
#12091 = CARTESIAN_POINT ( 'NONE',  ( -83.77821517812500929, -32.57812499938548711, 97.61286128772489690 ) ) ;
#12092 = CARTESIAN_POINT ( 'NONE',  ( -83.20395887649183919, -35.00000000000001421, -97.36341917746362640 ) ) ;
#12093 = CARTESIAN_POINT ( 'NONE',  ( 85.15643035625001289, -32.84062499938548285, 99.99999999999998579 ) ) ;
#12094 = FACE_OUTER_BOUND ( 'NONE', #15746, .T. ) ;
#12095 = DIRECTION ( 'NONE',  ( -0.000000000000000000, -1.000000000000000000, -0.000000000000000000 ) ) ;
#12096 = CARTESIAN_POINT ( 'NONE',  ( 79.39999999999999147, -34.21874999877096712, -99.99999999999998579 ) ) ;
#12097 = VECTOR ( 'NONE', #12553, 1000.000000000000114 ) ;
#12098 = CARTESIAN_POINT ( 'NONE',  ( 232.5999999999999375, -33.03749999999999432, 103.4641016151377499 ) ) ;
#12099 = ORIENTED_EDGE ( 'NONE', *, *, #10930, .T. ) ;
#12100 = CARTESIAN_POINT ( 'NONE',  ( 235.3564303562499447, -34.52812499938547575, -50.00000000000011369 ) ) ;
#12101 = DIRECTION ( 'NONE',  ( 1.838537592755934481E-31, 0.9242245927363030855, 0.3818493186865927203 ) ) ;
#12102 = CARTESIAN_POINT ( 'NONE',  ( 235.5999999999999375, -34.21874999877096002, 99.99999999999998579 ) ) ;
#12103 = CARTESIAN_POINT ( 'NONE',  ( 233.9782151781249411, -30.55312499938548143, -47.61286128772501769 ) ) ;
#12104 = EDGE_CURVE ( 'NONE', #5530, #2874, #8191, .T. ) ;
#12105 = CARTESIAN_POINT ( 'NONE',  ( -82.39999999999999147, -32.95312499938548711, 96.81714838363319586 ) ) ;
#12106 = TOROIDAL_SURFACE ( 'NONE', #12413, 5.384454397937118664, 0.5155456020628804703 ) ;
#12107 = VERTEX_POINT ( 'NONE', #10888 ) ;
#12108 = ORIENTED_EDGE ( 'NONE', *, *, #15340, .F. ) ;
#12109 = CARTESIAN_POINT ( 'NONE',  ( 231.0999999999999375, -32.71874999877096002, -52.59807621135342970 ) ) ;
#12110 = CARTESIAN_POINT ( 'NONE',  ( -80.90000000000000568, -34.14374999877097139, 97.40192378864668399 ) ) ;
#12111 = CARTESIAN_POINT ( 'NONE',  ( 4.151274195509471632, -4.079825909417648333, 5.067843131179045271E-16 ) ) ;
#12112 = ORIENTED_EDGE ( 'NONE', *, *, #3769, .T. ) ;
#12113 = CARTESIAN_POINT ( 'NONE',  ( 112.9999999999999858, -1.568190022283033361E-13, -2.720376046446971763E-29 ) ) ;
#12114 = CARTESIAN_POINT ( 'NONE',  ( 235.5999999999999375, -32.47499999999999432, 99.99999999999998579 ) ) ;
#12115 = AXIS2_PLACEMENT_3D ( 'NONE', #13485, #16526, #13774 ) ;
#12116 = AXIS2_PLACEMENT_3D ( 'NONE', #10481, #7455, #523 ) ;
#12117 = CARTESIAN_POINT ( 'NONE',  ( -79.64356964374999848, -34.52812499938548285, 99.99999999999998579 ) ) ;
#12118 = CARTESIAN_POINT ( 'NONE',  ( -85.40000000000000568, -30.37210047261201851, 100.9999487804559664 ) ) ;
#12119 = EDGE_CURVE ( 'NONE', #1583, #7197, #3000, .T. ) ;
#12120 = CARTESIAN_POINT ( 'NONE',  ( -83.90000000000000568, -31.66874999877096997, 102.5980762113533018 ) ) ;
#12121 = CARTESIAN_POINT ( 'NONE',  ( 244.7999999999999545, -4.999999999999976907, 150.0000000000000000 ) ) ;
#12122 = EDGE_CURVE ( 'NONE', #1594, #7899, #7699, .T. ) ;
#12123 = CARTESIAN_POINT ( 'NONE',  ( -79.39999999999999147, -33.82500000000000284, 99.99999999999998579 ) ) ;
#12124 = CARTESIAN_POINT ( 'NONE',  ( 3.974175853610081077, 2.726149789692974945, 2.409821656223290365 ) ) ;
#12125 = CARTESIAN_POINT ( 'NONE',  ( -82.40000000000000568, -34.78124999877096712, -96.99999999999998579 ) ) ;
#12126 = EDGE_CURVE ( 'NONE', #4990, #14525, #11426, .T. ) ;
#12127 = CARTESIAN_POINT ( 'NONE',  ( 229.8435696437499303, -31.49062499938547788, 99.99999999999998579 ) ) ;
#12128 = ORIENTED_EDGE ( 'NONE', *, *, #7013, .F. ) ;
#12129 = SURFACE_STYLE_FILL_AREA ( #9000 ) ;
#12130 = CARTESIAN_POINT ( 'NONE',  ( -82.39999999999999147, -32.50312499938548427, -103.1828516163667899 ) ) ;
#12131 = DIRECTION ( 'NONE',  ( -0.000000000000000000, -1.000000000000000000, -0.000000000000000000 ) ) ;
#12132 = FACE_OUTER_BOUND ( 'NONE', #16552, .T. ) ;
#12133 = CARTESIAN_POINT ( 'NONE',  ( 232.5999999999999375, -34.33124999877097139, 102.9999999999999858 ) ) ;
#12134 = CARTESIAN_POINT ( 'NONE',  ( 229.9986727058519307, -35.00000000000000711, -48.78874432549886819 ) ) ;
#12135 = CARTESIAN_POINT ( 'NONE',  ( 229.8435696437499303, -34.19062499938547717, -50.00000000000011369 ) ) ;
#12136 = VERTEX_POINT ( 'NONE', #6571 ) ;
#12137 = EDGE_LOOP ( 'NONE', ( #16984, #1521 ) ) ;
#12138 = DIRECTION ( 'NONE',  ( 0.000000000000000000, 0.000000000000000000, -1.000000000000000000 ) ) ;
#12139 = EDGE_CURVE ( 'NONE', #10188, #11820, #18610, .T. ) ;
#12140 = CARTESIAN_POINT ( 'NONE',  ( -82.39999999999999147, -31.68750000000000355, 103.4641016151377499 ) ) ;
#12141 = CARTESIAN_POINT ( 'NONE',  ( -82.39999999999999147, -32.53124999877096712, 103.4641016151377499 ) ) ;
#12142 = CARTESIAN_POINT ( 'NONE',  ( 83.90000000000000568, -31.87500000000000000, 102.5980762113533018 ) ) ;
#12143 = CARTESIAN_POINT ( 'NONE',  ( 83.90000000000000568, -33.46874999877096712, 97.40192378864668399 ) ) ;
#12144 = CARTESIAN_POINT ( 'NONE',  ( 235.3564303562499447, -34.90312499938547575, 101.5914258081833879 ) ) ;
#12145 =( BOUNDED_CURVE ( )  B_SPLINE_CURVE ( 2, ( #5447, #8451, #12558, #3672, #15982, #9638, #950, #8167, #6708 ),
 .UNSPECIFIED., .F., .F. ) 
 B_SPLINE_CURVE_WITH_KNOTS ( ( 3, 2, 2, 2, 3 ),
 ( 0.2291666666666666297, 0.2361111111111111049, 0.2500000000000000000, 0.2638888888888888951, 0.2708333333333333148 ),
 .UNSPECIFIED. ) 
 CURVE ( )  GEOMETRIC_REPRESENTATION_ITEM ( )  RATIONAL_B_SPLINE_CURVE ( ( 0.9330127018922194093, 0.9330127018922190762, 1.000000000000000000, 0.8660254037844387076, 1.000000000000000000, 0.8660254037844387076, 1.000000000000000000, 0.9330127018922196314, 0.9330127018922194093 ) ) 
 REPRESENTATION_ITEM ( '' )  );
#12146 = CARTESIAN_POINT ( 'NONE',  ( 82.39999999999999147, -33.29062499938548569, -103.1828516163667899 ) ) ;
#12147 = CARTESIAN_POINT ( 'NONE',  ( 80.07765479359947847, -32.00000000000000000, -98.15128725338327342 ) ) ;
#12148 = CARTESIAN_POINT ( 'NONE',  ( 79.64356964375001269, -34.90312499938548285, -101.5914258081833879 ) ) ;
#12149 = ORIENTED_EDGE ( 'NONE', *, *, #6792, .T. ) ;
#12150 = CARTESIAN_POINT ( 'NONE',  ( 231.0999999999999375, -31.87499999999999289, -52.59807621135342970 ) ) ;
#12151 = EDGE_CURVE ( 'NONE', #2374, #8719, #13996, .T. ) ;
#12152 = CARTESIAN_POINT ( 'NONE',  ( -81.59615242270662350, -31.61115380933863506, 102.9999999999999858 ) ) ;
#12153 = CARTESIAN_POINT ( 'NONE',  ( 81.02178482187500208, -33.89062499938548711, -97.61286128772489690 ) ) ;
#12154 = CARTESIAN_POINT ( 'NONE',  ( -2.100000000000000089, 2.571758278209441957E-16, -0.2800830152838844622 ) ) ;
#12155 = CARTESIAN_POINT ( 'NONE',  ( -81.02178482187500208, -31.75312499938548427, 97.61286128772489690 ) ) ;
#12156 = CARTESIAN_POINT ( 'NONE',  ( 232.5999999999999375, -33.74062499938548143, -46.81714838363331666 ) ) ;
#12157 = CARTESIAN_POINT ( 'NONE',  ( -80.90000000000000568, -30.15000000000000213, 97.40192378864668399 ) ) ;
#12158 = ORIENTED_EDGE ( 'NONE', *, *, #16274, .F. ) ;
#12159 = CARTESIAN_POINT ( 'NONE',  ( -79.96926199426660276, -35.00059217315788374, 101.7920197322231104 ) ) ;
#12160 = CARTESIAN_POINT ( 'NONE',  ( 229.8435696437499303, -33.74062499938548143, 99.99999999999998579 ) ) ;
#12161 = DIRECTION ( 'NONE',  ( 0.000000000000000000, 0.000000000000000000, -1.000000000000000000 ) ) ;
#12162 = CARTESIAN_POINT ( 'NONE',  ( -79.39999999999999147, -30.67500000000000071, 99.99999999999998579 ) ) ;
#12163 = CARTESIAN_POINT ( 'NONE',  ( 1.828356344711641102, 3.563200125723180900, -5.433716356636336675E-16 ) ) ;
#12164 = CARTESIAN_POINT ( 'NONE',  ( -85.15643035625001289, -30.29062499938548569, 98.40857419181659793 ) ) ;
#12165 = CARTESIAN_POINT ( 'NONE',  ( -79.39999999999999147, -32.88750000000000284, 98.26794919243110371 ) ) ;
#12166 = CARTESIAN_POINT ( 'NONE',  ( 85.15643035624999868, -34.34062499938548285, 101.5914258081833879 ) ) ;
#12167 = DIRECTION ( 'NONE',  ( 0.000000000000000000, -1.000000000000000000, 0.000000000000000000 ) ) ;
#12168 = CARTESIAN_POINT ( 'NONE',  ( 233.9782151781249411, -31.64062499938547646, -52.38713871227520968 ) ) ;
#12169 = CARTESIAN_POINT ( 'NONE',  ( -79.64356964374999848, -32.27812499938548996, 99.99999999999998579 ) ) ;
#12170 = CARTESIAN_POINT ( 'NONE',  ( -85.15643035625001289, -33.85312499938549280, -99.99999999999998579 ) ) ;
#12171 = PRODUCT_DEFINITION_CONTEXT ( 'detailed design', #19198, 'design' ) ;
#12172 = ORIENTED_EDGE ( 'NONE', *, *, #14147, .F. ) ;
#12173 = CARTESIAN_POINT ( 'NONE',  ( 82.39999999999999147, -34.78124999877096712, 96.53589838486223584 ) ) ;
#12174 = CARTESIAN_POINT ( 'NONE',  ( 82.40000000000000568, -34.78124999877096712, -102.9999999999999858 ) ) ;
#12175 = FILL_AREA_STYLE ('',( #18238 ) ) ;
#12176 = CARTESIAN_POINT ( 'NONE',  ( -79.64356964375001269, -31.34062499938548640, 98.40857419181659793 ) ) ;
#12177 = LINE ( 'NONE', #1818, #6193 ) ;
#12178 = ORIENTED_EDGE ( 'NONE', *, *, #6300, .F. ) ;
#12179 = CARTESIAN_POINT ( 'NONE',  ( -85.40000000000000568, -30.41249999999999787, -98.26794919243111792 ) ) ;
#12180 = CARTESIAN_POINT ( 'NONE',  ( 84.57144699476174310, -35.00000000000000000, 102.0792695867486657 ) ) ;
#12181 = CARTESIAN_POINT ( 'NONE',  ( 105.2000000000110020, -34.99999999999999289, -100.0000000000000000 ) ) ;
#12182 = CARTESIAN_POINT ( 'NONE',  ( -82.39999999999999147, -33.06562499938548427, -103.1828516163667899 ) ) ;
#12183 = CARTESIAN_POINT ( 'NONE',  ( -3.453038570459499024, -2.625189405340453419, -3.535263753545272891 ) ) ;
#12184 = CARTESIAN_POINT ( 'NONE',  ( 232.5999999999999375, -33.51562499938548001, 96.81714838363319586 ) ) ;
#12185 = CARTESIAN_POINT ( 'NONE',  ( -85.40000000000000568, -31.78518749875867400, 98.26794919243111792 ) ) ;
#12186 = ORIENTED_EDGE ( 'NONE', *, *, #16770, .T. ) ;
#12187 = DIRECTION ( 'NONE',  ( 1.000000000000000000, -4.625929269271524001E-17, -6.308085367188448025E-15 ) ) ;
#12188 = CARTESIAN_POINT ( 'NONE',  ( 81.02178482187500208, -32.69062499938548427, 97.61286128772489690 ) ) ;
#12189 = LINE ( 'NONE', #10723, #2755 ) ;
#12190 = DIRECTION ( 'NONE',  ( 0.000000000000000000, -1.000000000000000000, 0.000000000000000000 ) ) ;
#12191 = CARTESIAN_POINT ( 'NONE',  ( 79.39999999999999147, -33.73124999877096997, -98.26794919243110371 ) ) ;
#12192 = CARTESIAN_POINT ( 'NONE',  ( 234.0999999999999375, -33.74999999999999289, 97.40192378864668399 ) ) ;
#12193 = ORIENTED_EDGE ( 'NONE', *, *, #12336, .F. ) ;
#12194 = CARTESIAN_POINT ( 'NONE',  ( 235.3564303562499447, -33.59062499938547575, -51.59142580818350154 ) ) ;
#12195 = CARTESIAN_POINT ( 'NONE',  ( 314.9999999999999432, 6.938893903907228378E-15, -1.665334536937739347E-15 ) ) ;
#12196 = CARTESIAN_POINT ( 'NONE',  ( 229.5999999999999375, -35.30624999877095860, 101.7320508075688679 ) ) ;
#12197 = CARTESIAN_POINT ( 'NONE',  ( 231.0999999999999375, -34.81874999877096144, -47.40192378864679768 ) ) ;
#12198 =( REPRESENTATION_RELATIONSHIP ('NONE','NONE', #14468, #9634 ) REPRESENTATION_RELATIONSHIP_WITH_TRANSFORMATION ( #14329 )SHAPE_REPRESENTATION_RELATIONSHIP( ) );
#12199 = DIRECTION ( 'NONE',  ( 0.000000000000000000, 0.000000000000000000, 1.000000000000000000 ) ) ;
#12200 = ORIENTED_EDGE ( 'NONE', *, *, #15121, .F. ) ;
#12201 = ORIENTED_EDGE ( 'NONE', *, *, #12713, .F. ) ;
#12202 = CARTESIAN_POINT ( 'NONE',  ( -79.64356964375001269, -30.32812499938548711, -101.5914258081833879 ) ) ;
#12203 = CARTESIAN_POINT ( 'NONE',  ( -79.39999999999999147, -34.21874999877096712, 99.99999999999998579 ) ) ;
#12204 = CARTESIAN_POINT ( 'NONE',  ( 4.165266963751926177, -4.099263933823847239, 5.067843131179045271E-16 ) ) ;
#12205 = ORIENTED_EDGE ( 'NONE', *, *, #8320, .F. ) ;
#12206 = CARTESIAN_POINT ( 'NONE',  ( 113.0000000000000000, 10.19999999999997264, -139.9999999999999716 ) ) ;
#12207 = CARTESIAN_POINT ( 'NONE',  ( -82.39999999999999147, -34.83749999999999858, 103.0000000000000000 ) ) ;
#12208 = ADVANCED_FACE ( 'NONE', ( #6867 ), #18588, .F. ) ;
#12209 = CARTESIAN_POINT ( 'NONE',  ( -81.59615242270662350, -34.36740381056766580, 102.9999999999999858 ) ) ;
#12210 = CARTESIAN_POINT ( 'NONE',  ( -83.90000000000000568, -30.46874999877096712, 97.40192378864668399 ) ) ;
#12211 = CARTESIAN_POINT ( 'NONE',  ( -85.40000000000000568, -32.15624999877096712, 101.7320508075688679 ) ) ;
#12212 = FACE_OUTER_BOUND ( 'NONE', #8314, .T. ) ;
#12213 = ADVANCED_FACE ( 'NONE', ( #8025 ), #6769, .T. ) ;
#12214 = ADVANCED_FACE ( 'NONE', ( #623 ), #5305, .T. ) ;
#12215 = CARTESIAN_POINT ( 'NONE',  ( 111.5000000000000142, 12.69999999999998508, 110.0000000000000142 ) ) ;
#12216 = CARTESIAN_POINT ( 'NONE',  ( 81.59615242270665192, -34.81740381056767575, -103.0000000000000000 ) ) ;
#12217 = CYLINDRICAL_SURFACE ( 'NONE', #5279, 3.000000000000009770 ) ;
#12218 = CARTESIAN_POINT ( 'NONE',  ( 233.9782151781249411, -31.79062499938548214, 102.3871387122750889 ) ) ;
#12219 = VERTEX_POINT ( 'NONE', #9691 ) ;
#12220 = CARTESIAN_POINT ( 'NONE',  ( -82.39999999999999147, -33.40312499938548285, -103.1828516163667899 ) ) ;
#12221 = CARTESIAN_POINT ( 'NONE',  ( 4.082498951862917558, 4.041451884327382338, 2.013392555975283473E-32 ) ) ;
#12222 = VERTEX_POINT ( 'NONE', #17213 ) ;
#12223 = FACE_BOUND ( 'NONE', #15279, .T. ) ;
#12224 = CARTESIAN_POINT ( 'NONE',  ( 83.20395887649171129, -35.00000000000000711, -102.6365808225363878 ) ) ;
#12225 = CARTESIAN_POINT ( 'NONE',  ( 230.0248882325211923, -35.00000000000002132, -51.51699773205431399 ) ) ;
#12226 = FACE_OUTER_BOUND ( 'NONE', #10639, .T. ) ;
#12227 = AXIS2_PLACEMENT_3D ( 'NONE', #6884, #17329, #9617 ) ;
#12228 =( GEOMETRIC_REPRESENTATION_CONTEXT ( 3 ) GLOBAL_UNCERTAINTY_ASSIGNED_CONTEXT ( ( #5310 ) ) GLOBAL_UNIT_ASSIGNED_CONTEXT ( ( #9085, #5975, #10460 ) ) REPRESENTATION_CONTEXT ( 'NONE', 'WORKASPACE' ) );
#12230 = ADVANCED_FACE ( 'NONE', ( #3818 ), #15557, .F. ) ;
#12229 = VERTEX_POINT ( 'NONE', #16833 ) ;
#12231 = VERTEX_POINT ( 'NONE', #8317 ) ;
#12232 = CARTESIAN_POINT ( 'NONE',  ( -80.24533121543032621, -32.00000000000001421, 102.0417045141624044 ) ) ;
#12233 = CARTESIAN_POINT ( 'NONE',  ( 80.90000000000000568, -31.05000000000000071, -97.40192378864668399 ) ) ;
#12234 = EDGE_CURVE ( 'NONE', #10401, #2299, #7931, .T. ) ;
#12235 = ADVANCED_FACE ( 'NONE', ( #5202 ), #8228, .F. ) ;
#12236 = CARTESIAN_POINT ( 'NONE',  ( -80.90000000000000568, -31.59374999877097423, 102.5980762113533018 ) ) ;
#12237 = CARTESIAN_POINT ( 'NONE',  ( 85.40000000000000568, -31.31250000000000000, 98.26794919243111792 ) ) ;
#12238 = CARTESIAN_POINT ( 'NONE',  ( -84.44763168836720979, -32.00000000000001421, -98.15470523285542015 ) ) ;
#12239 = CARTESIAN_POINT ( 'NONE',  ( 233.9782151781249411, -34.94062499938547717, 102.3871387122750889 ) ) ;
#12240 = CARTESIAN_POINT ( 'NONE',  ( 82.39999999999999147, -34.19062499938548427, -103.1828516163667899 ) ) ;
#12241 = CARTESIAN_POINT ( 'NONE',  ( 0.000000000000000000, 0.000000000000000000, 0.000000000000000000 ) ) ;
#12242 = AXIS2_PLACEMENT_3D ( 'NONE', #14852, #16709, #4805 ) ;
#12243 = VECTOR ( 'NONE', #9748, 1000.000000000000000 ) ;
#12244 = CARTESIAN_POINT ( 'NONE',  ( 85.15643035625001289, -33.74062499938548854, -99.99999999999998579 ) ) ;
#12245 = ORIENTED_EDGE ( 'NONE', *, *, #18668, .T. ) ;
#12246 = CARTESIAN_POINT ( 'NONE',  ( 235.5999999999999375, -33.82499999999999574, -50.00000000000011369 ) ) ;
#12247 = CARTESIAN_POINT ( 'NONE',  ( 85.15643035625001289, -32.39062499938548711, -99.99999999999998579 ) ) ;
#12248 = CARTESIAN_POINT ( 'NONE',  ( -83.33080762004576059, -35.05289549976084373, 96.44210921874548603 ) ) ;
#12249 = DIRECTION ( 'NONE',  ( -0.000000000000000000, 1.000000000000000000, 0.000000000000000000 ) ) ;
#12250 = CARTESIAN_POINT ( 'NONE',  ( -85.15643035624999868, -30.66562499938548569, 101.5914258081833879 ) ) ;
#12251 = CARTESIAN_POINT ( 'NONE',  ( 233.9782151781249411, -34.15312499938547575, -47.61286128772501769 ) ) ;
#12252 = CARTESIAN_POINT ( 'NONE',  ( -85.40000000000000568, -30.93750000000000355, 98.26794919243111792 ) ) ;
#12253 = ORIENTED_EDGE ( 'NONE', *, *, #11986, .F. ) ;
#12254 = CARTESIAN_POINT ( 'NONE',  ( -80.42875664086302834, -34.99897389098457978, 97.71408729985186881 ) ) ;
#12255 = VECTOR ( 'NONE', #2735, 1000.000000000000000 ) ;
#12256 =( BOUNDED_CURVE ( )  B_SPLINE_CURVE ( 2, ( #3125, #24, #15048, #13391, #214, #6171, #7623, #13576, #18091 ),
 .UNSPECIFIED., .F., .F. ) 
 B_SPLINE_CURVE_WITH_KNOTS ( ( 3, 2, 2, 2, 3 ),
 ( 0.6458333333333332593, 0.6527777777777777901, 0.6666666666666666297, 0.6805555555555555802, 0.6875000000000000000 ),
 .UNSPECIFIED. ) 
 CURVE ( )  GEOMETRIC_REPRESENTATION_ITEM ( )  RATIONAL_B_SPLINE_CURVE ( ( 0.9330127018922192983, 0.9330127018922187432, 1.000000000000000000, 0.8660254037844387076, 1.000000000000000000, 0.8660254037844387076, 1.000000000000000000, 0.9330127018922194093, 0.9330127018922194093 ) ) 
 REPRESENTATION_ITEM ( '' )  );
#12257 = AXIS2_PLACEMENT_3D ( 'NONE', #4439, #12249, #10397 ) ;
#12258 = CARTESIAN_POINT ( 'NONE',  ( -82.40000000000001990, -34.16250000000000853, 97.00000000000000000 ) ) ;
#12259 = EDGE_CURVE ( 'NONE', #10850, #12903, #16567, .T. ) ;
#12260 = CARTESIAN_POINT ( 'NONE',  ( 82.39999999999999147, -30.70312499938548711, 103.1828516163667899 ) ) ;
#12261 = EDGE_CURVE ( 'NONE', #17075, #1272, #5335, .T. ) ;
#12262 = CARTESIAN_POINT ( 'NONE',  ( 230.3249173797030096, -32.00000000000000000, -48.43364869553379037 ) ) ;
#12263 = CARTESIAN_POINT ( 'NONE',  ( -85.15643035625001289, -31.15312499938548996, 99.99999999999998579 ) ) ;
#12264 = CARTESIAN_POINT ( 'NONE',  ( 4.050880675075949178, 1.379097446046194220, 3.567934390854430760 ) ) ;
#12265 = CARTESIAN_POINT ( 'NONE',  ( 79.64356964375001269, -30.85312499938548569, 98.40857419181659793 ) ) ;
#12266 = CARTESIAN_POINT ( 'NONE',  ( 79.64356964375001269, -32.69062499938548427, -98.40857419181659793 ) ) ;
#12267 = ADVANCED_FACE ( 'NONE', ( #16925 ), #15653, .F. ) ;
#12268 = CARTESIAN_POINT ( 'NONE',  ( 229.8435696437499871, -30.55312499938547788, -48.40857419181671162 ) ) ;
#12269 = CARTESIAN_POINT ( 'NONE',  ( -81.02178482187500208, -34.15312499938548285, 102.3871387122750889 ) ) ;
#12270 = CARTESIAN_POINT ( 'NONE',  ( -81.02178482187500208, -33.10312499938548569, -102.3871387122750889 ) ) ;
#12271 = AXIS2_PLACEMENT_3D ( 'NONE', #13880, #7834, #519 ) ;
#12272 = ORIENTED_EDGE ( 'NONE', *, *, #5306, .F. ) ;
#12273 = CARTESIAN_POINT ( 'NONE',  ( 85.15643035625001289, -30.25312499938548783, 99.99999999999998579 ) ) ;
#12274 = CARTESIAN_POINT ( 'NONE',  ( 234.0999999999999375, -34.35000000000000142, 102.5980762113533018 ) ) ;
#12275 = CARTESIAN_POINT ( 'NONE',  ( 4.132952817037860882, -2.031684012687265284, -3.518979934899746365 ) ) ;
#12276 = CARTESIAN_POINT ( 'NONE',  ( -79.64356964375001269, -34.94062499938549138, 98.40857419181659793 ) ) ;
#12277 = LINE ( 'NONE', #18240, #572 ) ;
#12278 = ORIENTED_EDGE ( 'NONE', *, *, #3028, .T. ) ;
#12279 = CARTESIAN_POINT ( 'NONE',  ( -82.39999999999999147, -31.23750000000000071, -96.53589838486223584 ) ) ;
#12280 = CARTESIAN_POINT ( 'NONE',  ( 83.90000000000000568, -34.57500000000000284, -97.40192378864668399 ) ) ;
#12281 = DIRECTION ( 'NONE',  ( -1.000000000000000000, 0.000000000000000000, 0.000000000000000000 ) ) ;
#12282 = CARTESIAN_POINT ( 'NONE',  ( -81.02178482187500208, -35.05312499938548854, -97.61286128772489690 ) ) ;
#12283 = CARTESIAN_POINT ( 'NONE',  ( -2.756197834950067094, -3.027510591568735254, -3.223146290109809797 ) ) ;
#12284 = CARTESIAN_POINT ( 'NONE',  ( 235.3564303562499447, -33.14062499938548001, 98.40857419181659793 ) ) ;
#12285 = CARTESIAN_POINT ( 'NONE',  ( -79.39999999999999147, -34.18518749875867258, 98.26794919243110371 ) ) ;
#12286 = ORIENTED_EDGE ( 'NONE', *, *, #10564, .T. ) ;
#12287 = CARTESIAN_POINT ( 'NONE',  ( 229.5999999999999375, -32.73749999999999716, 98.26794919243111792 ) ) ;
#12288 = CARTESIAN_POINT ( 'NONE',  ( 80.90000000000000568, -32.79374999877096997, -97.40192378864668399 ) ) ;
#12289 = CARTESIAN_POINT ( 'NONE',  ( 81.02178482187500208, -32.24062499938548854, 97.61286128772489690 ) ) ;
#12290 = PLANE ( 'NONE',  #13045 ) ;
#12291 = CARTESIAN_POINT ( 'NONE',  ( -85.40000000000000568, -34.40624999877096712, 101.7320508075688821 ) ) ;
#12292 = CARTESIAN_POINT ( 'NONE',  ( 80.90000000000000568, -34.74374999877097281, -102.5980762113533018 ) ) ;
#12293 = DIRECTION ( 'NONE',  ( -0.000000000000000000, -0.000000000000000000, 1.000000000000000000 ) ) ;
#12294 = ORIENTED_EDGE ( 'NONE', *, *, #6502, .T. ) ;
#12295 = CARTESIAN_POINT ( 'NONE',  ( 235.3564303562499447, -33.17812499938548143, -50.00000000000011369 ) ) ;
#12296 = DIRECTION ( 'NONE',  ( 0.000000000000000000, 0.000000000000000000, 1.000000000000000000 ) ) ;
#12297 = CARTESIAN_POINT ( 'NONE',  ( 229.8435696437499303, -32.50312499938547717, 99.99999999999998579 ) ) ;
#12298 = CARTESIAN_POINT ( 'NONE',  ( 229.5999999999999943, -35.36739044046695568, -51.09190523015522700 ) ) ;
#12299 = CARTESIAN_POINT ( 'NONE',  ( -82.39999999999999147, -34.97812499938548569, 103.1828516163667899 ) ) ;
#12300 = VERTEX_POINT ( 'NONE', #2636 ) ;
#12301 = EDGE_LOOP ( 'NONE', ( #15116, #3247, #112 ) ) ;
#12302 = CARTESIAN_POINT ( 'NONE',  ( 4.024499207728848837, 2.323545700935681246, -3.572172305156870564 ) ) ;
#12303 = CARTESIAN_POINT ( 'NONE',  ( -83.90000000000000568, -32.32500000000000284, -102.5980762113533018 ) ) ;
#12304 = PLANE ( 'NONE',  #82 ) ;
#12305 = EDGE_LOOP ( 'NONE', ( #2079, #7394 ) ) ;
#12306 = CARTESIAN_POINT ( 'NONE',  ( -85.40000000000000568, -31.29374999877096997, 99.99999999999998579 ) ) ;
#12307 = CARTESIAN_POINT ( 'NONE',  ( -79.39999999999999147, -33.35624999877097707, -98.26794919243113213 ) ) ;
#12308 = CARTESIAN_POINT ( 'NONE',  ( -82.40000000000000568, -30.00000000000000355, 96.99999999999998579 ) ) ;
#12309 = CARTESIAN_POINT ( 'NONE',  ( -82.39999999999999147, -30.73124999877096641, 103.4641016151377499 ) ) ;
#12310 = CARTESIAN_POINT ( 'NONE',  ( -85.40000000000000568, -34.89374999877097139, 99.99999999999998579 ) ) ;
#12311 = CARTESIAN_POINT ( 'NONE',  ( 0.000000000000000000, 0.000000000000000000, 0.000000000000000000 ) ) ;
#12312 = CARTESIAN_POINT ( 'NONE',  ( 80.90000000000000568, -34.14374999877097139, -97.40192378864668399 ) ) ;
#12313 = SURFACE_SIDE_STYLE ('',( #15337 ) ) ;
#12314 = CARTESIAN_POINT ( 'NONE',  ( 105.1999999999999744, -31.99999999999999289, 153.0000000000000000 ) ) ;
#12315 = CARTESIAN_POINT ( 'NONE',  ( 233.9782151781249411, -33.44062499938547717, 97.61286128772489690 ) ) ;
#12316 = CARTESIAN_POINT ( 'NONE',  ( 233.9782151781249411, -32.69062499938547717, 102.3871387122750889 ) ) ;
#12317 = VERTEX_POINT ( 'NONE', #11346 ) ;
#12318 =( NAMED_UNIT ( * ) PLANE_ANGLE_UNIT ( ) SI_UNIT ( $, .RADIAN. ) );
#12319 = CARTESIAN_POINT ( 'NONE',  ( -79.64356964375001269, -34.00312499938549138, -98.40857419181659793 ) ) ;
#12320 = CARTESIAN_POINT ( 'NONE',  ( 229.5999999999999375, -32.15624999877096002, 101.7320508075688821 ) ) ;
#12321 = EDGE_LOOP ( 'NONE', ( #18271, #12782, #9681, #10953 ) ) ;
#12322 = CARTESIAN_POINT ( 'NONE',  ( -4.211140560182196957, -2.431303136016552013, -3.745885042887436178 ) ) ;
#12323 = CARTESIAN_POINT ( 'NONE',  ( -2.688821387764050996E-14, -4.618802153517012954, -0.4999999999999995559 ) ) ;
#12324 = CARTESIAN_POINT ( 'NONE',  ( 4.000000000000000000, 0.7924765000094659007, -0.05906175389889852662 ) ) ;
#12325 = ORIENTED_EDGE ( 'NONE', *, *, #14019, .T. ) ;
#12326 = CARTESIAN_POINT ( 'NONE',  ( 229.8435696437499871, -34.67812499938547433, -51.59142580818350865 ) ) ;
#12327 = EDGE_CURVE ( 'NONE', #9376, #12074, #7146, .T. ) ;
#12328 = ORIENTED_EDGE ( 'NONE', *, *, #5910, .F. ) ;
#12329 = EDGE_LOOP ( 'NONE', ( #18751, #2248, #15626, #13647 ) ) ;
#12330 = CARTESIAN_POINT ( 'NONE',  ( 80.90000000000000568, -33.39374999877097139, -102.5980762113533018 ) ) ;
#12331 = CARTESIAN_POINT ( 'NONE',  ( 83.88339518848731302, -35.16733441503058089, -97.47959136244114120 ) ) ;
#12332 = CARTESIAN_POINT ( 'NONE',  ( -82.39999999999999147, -34.78124999877096712, 103.4641016151377499 ) ) ;
#12333 = CARTESIAN_POINT ( 'NONE',  ( -82.40000000000001990, -34.16250000000000853, -103.0000000000000000 ) ) ;
#12334 = CARTESIAN_POINT ( 'NONE',  ( -4.000000000000000000, 2.309401076758498483, -0.4999999999999927280 ) ) ;
#12335 = CARTESIAN_POINT ( 'NONE',  ( 82.39999999999999147, -32.16562499938548569, -96.81714838363319586 ) ) ;
#12336 = EDGE_CURVE ( 'NONE', #13758, #13209, #15846, .T. ) ;
#12337 = DIRECTION ( 'NONE',  ( 1.000000000000000000, -1.156482317317870344E-15, 0.000000000000000000 ) ) ;
#12338 = CARTESIAN_POINT ( 'NONE',  ( -79.64356964375001269, -33.02812499938548285, 98.40857419181659793 ) ) ;
#12339 = VECTOR ( 'NONE', #7522, 1000.000000000000000 ) ;
#12340 = EDGE_CURVE ( 'NONE', #104, #10751, #1288, .T. ) ;
#12341 = CARTESIAN_POINT ( 'NONE',  ( 79.64356964375001269, -33.92812499938548854, -98.40857419181659793 ) ) ;
#12342 = ORIENTED_EDGE ( 'NONE', *, *, #4577, .T. ) ;
#12343 = CARTESIAN_POINT ( 'NONE',  ( 235.5999999999999375, -31.57499999999999218, -50.00000000000011369 ) ) ;
#12344 = CARTESIAN_POINT ( 'NONE',  ( -94.79999999999999716, -32.00000000000000000, 150.0000000000000000 ) ) ;
#12345 = CARTESIAN_POINT ( 'NONE',  ( 94.79999999999995453, -29.80000000000000071, 150.0000000000000000 ) ) ;
#12346 = DIRECTION ( 'NONE',  ( -0.000000000000000000, -1.000000000000000000, -0.000000000000000000 ) ) ;
#12347 = CARTESIAN_POINT ( 'NONE',  ( -79.64356964375001269, -30.96562499938548640, 101.5914258081833879 ) ) ;
#12348 = CARTESIAN_POINT ( 'NONE',  ( 229.8435696437499303, -32.95312499938548001, -50.00000000000011369 ) ) ;
#12349 = CARTESIAN_POINT ( 'NONE',  ( -83.90000000000000568, -31.87500000000000000, 97.40192378864668399 ) ) ;
#12350 = ADVANCED_FACE ( 'NONE', ( #9983 ), #11445, .F. ) ;
#12351 = EDGE_LOOP ( 'NONE', ( #2786, #4173, #13256, #11417 ) ) ;
#12352 = CARTESIAN_POINT ( 'NONE',  ( -80.84132516849733463, -34.99999918353109507, 97.43127812267456989 ) ) ;
#12353 = VECTOR ( 'NONE', #6330, 1000.000000000000000 ) ;
#12354 = CARTESIAN_POINT ( 'NONE',  ( 3.973514160553461849, 2.741076955031360285, 2.383932505289870996 ) ) ;
#12355 = CARTESIAN_POINT ( 'NONE',  ( 229.8787539177867814, -32.00000000000002132, -50.47355695758027139 ) ) ;
#12356 = CARTESIAN_POINT ( 'NONE',  ( -82.39999999999999147, -30.36562499938548854, 96.81714838363319586 ) ) ;
#12357 = CARTESIAN_POINT ( 'NONE',  ( -79.64356964374999848, -32.27812499938548996, -99.99999999999998579 ) ) ;
#12358 = CARTESIAN_POINT ( 'NONE',  ( 81.02178482187500208, -34.00312499938548427, 102.3871387122750889 ) ) ;
#12359 = COLOUR_RGB ( '',0.8941176470588234615, 0.8941176470588234615, 0.8941176470588234615 ) ;
#12360 = EDGE_CURVE ( 'NONE', #2207, #3690, #3513, .T. ) ;
#12361 = CARTESIAN_POINT ( 'NONE',  ( 83.77821517812500929, -32.42812499938548854, -102.3871387122750889 ) ) ;
#12362 = CARTESIAN_POINT ( 'NONE',  ( 232.5999999999999375, -30.92812499938547433, -46.81714838363331666 ) ) ;
#12363 = CARTESIAN_POINT ( 'NONE',  ( -83.77821517812500929, -34.37812499938548427, 97.61286128772489690 ) ) ;
#12364 = CARTESIAN_POINT ( 'NONE',  ( -83.77821517812500929, -32.87812499938548427, -97.61286128772489690 ) ) ;
#12365 = AXIS2_PLACEMENT_3D ( 'NONE', #18086, #7426, #6166 ) ;
#12366 = ORIENTED_EDGE ( 'NONE', *, *, #2320, .T. ) ;
#12367 = CARTESIAN_POINT ( 'NONE',  ( 85.15643035624999868, -31.64062499938548356, 101.5914258081833879 ) ) ;
#12368 = DIRECTION ( 'NONE',  ( 0.8191520442889875797, 0.000000000000000000, 0.5735764363510522656 ) ) ;
#12369 =( BOUNDED_CURVE ( )  B_SPLINE_CURVE ( 2, ( #12530, #9604, #15569, #2467, #6877 ),
 .UNSPECIFIED., .F., .F. ) 
 B_SPLINE_CURVE_WITH_KNOTS ( ( 3, 2, 3 ),
 ( 0.2975293541897500171, 0.3055555555555555802, 0.3125000000000000555 ),
 .UNSPECIFIED. ) 
 CURVE ( )  GEOMETRIC_REPRESENTATION_ITEM ( )  RATIONAL_B_SPLINE_CURVE ( ( 0.9346381638529870362, 0.9225778897267418177, 1.000000000000000000, 0.9330127018922187432, 0.9330127018922192983 ) ) 
 REPRESENTATION_ITEM ( '' )  );
#12370 = CARTESIAN_POINT ( 'NONE',  ( -85.15643035624999868, -33.44062499938548427, 98.40857419181659793 ) ) ;
#12371 = CARTESIAN_POINT ( 'NONE',  ( 235.5999999999999375, -32.02499999999999858, -50.00000000000011369 ) ) ;
#12372 = VERTEX_POINT ( 'NONE', #11726 ) ;
#12373 = CARTESIAN_POINT ( 'NONE',  ( -79.39999999999999147, -31.16250000000000497, -98.26794919243113213 ) ) ;
#12374 = CARTESIAN_POINT ( 'NONE',  ( 84.42750213138106119, -35.00000000000000000, 102.2200415044236905 ) ) ;
#12375 = PLANE ( 'NONE',  #10771 ) ;
#12376 = EDGE_CURVE ( 'NONE', #17929, #3617, #2825, .T. ) ;
#12377 = DIRECTION ( 'NONE',  ( -0.000000000000000000, -1.000000000000000000, -0.000000000000000000 ) ) ;
#12378 = CARTESIAN_POINT ( 'NONE',  ( -2.500000000000000444, 3.061616997868383634E-16, -5.000000000000000888 ) ) ;
#12379 = CARTESIAN_POINT ( 'NONE',  ( 229.8435696437499871, -34.71562499938548285, 101.5914258081833879 ) ) ;
#12380 = CARTESIAN_POINT ( 'NONE',  ( -79.39999999999999147, -33.77268749875867826, 99.99999999999998579 ) ) ;
#12381 = VERTEX_POINT ( 'NONE', #17504 ) ;
#12382 = DIRECTION ( 'NONE',  ( 0.000000000000000000, 1.000000000000000000, 0.000000000000000000 ) ) ;
#12383 = CARTESIAN_POINT ( 'NONE',  ( -83.90000000000000568, -33.22500000000000142, 97.40192378864668399 ) ) ;
#12384 = CARTESIAN_POINT ( 'NONE',  ( -94.79999999999999716, -5.200000000000000178, 150.0000000000000000 ) ) ;
#12385 = CARTESIAN_POINT ( 'NONE',  ( -82.39999999999999147, -31.23750000000000071, 102.9999999999999858 ) ) ;
#12386 = CARTESIAN_POINT ( 'NONE',  ( 79.64356964374999848, -30.92812499938548498, -99.99999999999998579 ) ) ;
#12387 = CARTESIAN_POINT ( 'NONE',  ( 25.60000000000000142, 0.000000000000000000, 0.000000000000000000 ) ) ;
#12388 = ORIENTED_EDGE ( 'NONE', *, *, #14122, .F. ) ;
#12389 = CARTESIAN_POINT ( 'NONE',  ( 5.599999999999999645, 2.020725942163688504, 3.500000000000000000 ) ) ;
#12390 = CARTESIAN_POINT ( 'NONE',  ( 232.5999999999999375, -32.84062499938548285, 103.1828516163667899 ) ) ;
#12391 = CARTESIAN_POINT ( 'NONE',  ( 229.8435696437499303, -31.60312499938548214, -50.00000000000011369 ) ) ;
#12392 = VECTOR ( 'NONE', #2128, 1000.000000000000000 ) ;
#12393 = CARTESIAN_POINT ( 'NONE',  ( -83.77821517812500929, -33.81562499938548427, 97.61286128772489690 ) ) ;
#12394 = DIRECTION ( 'NONE',  ( 1.000000000000000000, -0.000000000000000000, -2.407412430484046130E-31 ) ) ;
#12395 = EDGE_LOOP ( 'NONE', ( #10548, #9574, #2272, #18463, #10264, #13759 ) ) ;
#12396 = VERTEX_POINT ( 'NONE', #10273 ) ;
#12397 = CARTESIAN_POINT ( 'NONE',  ( 231.7961524227065695, -32.73615380933862440, -53.00000000000012079 ) ) ;
#12398 = CARTESIAN_POINT ( 'NONE',  ( 232.5999999999999375, -29.99999999999999645, -50.00000000000011369 ) ) ;
#12399 = CARTESIAN_POINT ( 'NONE',  ( -82.40000000000000568, -33.71249999999998437, -102.9999999999999858 ) ) ;
#12400 = ORIENTED_EDGE ( 'NONE', *, *, #17619, .F. ) ;
#12401 = DIRECTION ( 'NONE',  ( 2.407412430484046130E-31, -3.340955887615246502E-46, 1.000000000000000000 ) ) ;
#12402 = CONICAL_SURFACE ( 'NONE', #4611, 3.500000000000000000, 1.047197551196600296 ) ;
#12403 = CARTESIAN_POINT ( 'NONE',  ( -79.39999999999999147, -34.70624999877097139, -98.26794919243113213 ) ) ;
#12404 = CARTESIAN_POINT ( 'NONE',  ( -2.682243648011671588, -3.070208061305317759, -0.04852650426602272971 ) ) ;
#12405 = CARTESIAN_POINT ( 'NONE',  ( -83.90000000000000568, -33.01874999877097139, 102.5980762113533018 ) ) ;
#12406 = CARTESIAN_POINT ( 'NONE',  ( -82.39999999999999147, -34.10624999877096997, 96.53589838486223584 ) ) ;
#12407 = AXIS2_PLACEMENT_3D ( 'NONE', #13104, #14857, #17899 ) ;
#12408 = CARTESIAN_POINT ( 'NONE',  ( -79.39999999999999147, -30.65624999877096712, 101.7320508075688537 ) ) ;
#12409 = FACE_OUTER_BOUND ( 'NONE', #7117, .T. ) ;
#12410 = FACE_OUTER_BOUND ( 'NONE', #5963, .T. ) ;
#12411 = CARTESIAN_POINT ( 'NONE',  ( 232.5999999999999375, -33.17812499938548143, 103.1828516163667899 ) ) ;
#12412 = ORIENTED_EDGE ( 'NONE', *, *, #17331, .T. ) ;
#12413 = AXIS2_PLACEMENT_3D ( 'NONE', #8221, #5101, #1965 ) ;
#12414 = CARTESIAN_POINT ( 'NONE',  ( 232.5999999999999375, -30.95624999877096428, 96.53589838486223584 ) ) ;
#12415 = CARTESIAN_POINT ( 'NONE',  ( 102.9999999999999858, -29.80000000000000071, 150.0000000000000000 ) ) ;
#12416 = VERTEX_POINT ( 'NONE', #2741 ) ;
#12417 = CARTESIAN_POINT ( 'NONE',  ( -82.39999999999999147, -33.48750000000000426, -97.00000000000000000 ) ) ;
#12418 = CARTESIAN_POINT ( 'NONE',  ( 0.3126073911695752550, -2.020725942163798194, -3.500000000000000000 ) ) ;
#12419 = CARTESIAN_POINT ( 'NONE',  ( 3.999999999999999112, 1.941961291383486277, -0.3515519931180248192 ) ) ;
#12420 = ORIENTED_EDGE ( 'NONE', *, *, #5720, .F. ) ;
#12421 = CARTESIAN_POINT ( 'NONE',  ( 229.5999999999999375, -33.58124999877096428, 98.26794919243111792 ) ) ;
#12422 = AXIS2_PLACEMENT_3D ( 'NONE', #10253, #15027, #17778 ) ;
#12423 = VECTOR ( 'NONE', #18252, 1000.000000000000000 ) ;
#12424 = ORIENTED_EDGE ( 'NONE', *, *, #13900, .F. ) ;
#12425 = ORIENTED_EDGE ( 'NONE', *, *, #2265, .F. ) ;
#12426 = CARTESIAN_POINT ( 'NONE',  ( 235.5999999999999375, -33.37499999999999289, -50.00000000000011369 ) ) ;
#12427 = CARTESIAN_POINT ( 'NONE',  ( 79.39999999999999147, -31.53750000000000497, -98.26794919243110371 ) ) ;
#12428 = DIRECTION ( 'NONE',  ( 0.000000000000000000, 0.000000000000000000, -1.000000000000000000 ) ) ;
#12429 = CARTESIAN_POINT ( 'NONE',  ( -80.90000000000000568, -33.84374999877096712, 102.5980762113533018 ) ) ;
#12430 = CIRCLE ( 'NONE', #18482, 2.649999999999982148 ) ;
#12431 = CARTESIAN_POINT ( 'NONE',  ( 85.40000000000000568, -32.21250000000000568, -101.7320508075688821 ) ) ;
#12432 = CARTESIAN_POINT ( 'NONE',  ( 79.64356964374999848, -34.07812499938548711, -99.99999999999998579 ) ) ;
#12433 = CARTESIAN_POINT ( 'NONE',  ( 80.90000000000000568, -33.30000000000000426, -97.40192378864668399 ) ) ;
#12434 = CARTESIAN_POINT ( 'NONE',  ( -81.02178482187500208, -32.99062499938548854, 97.61286128772489690 ) ) ;
#12435 = CARTESIAN_POINT ( 'NONE',  ( 83.77821517812500929, -32.76562499938548711, -102.3871387122750889 ) ) ;
#12436 = ORIENTED_EDGE ( 'NONE', *, *, #6388, .F. ) ;
#12437 = CARTESIAN_POINT ( 'NONE',  ( 229.5999999999999375, -31.79999999999999361, -50.00000000000011369 ) ) ;
#12438 = CARTESIAN_POINT ( 'NONE',  ( -80.90000000000000568, -34.64999999999999858, 97.40192378864668399 ) ) ;
#12439 = CARTESIAN_POINT ( 'NONE',  ( 82.40000000000001990, -32.13750000000000284, 97.00000000000000000 ) ) ;
#12440 = CARTESIAN_POINT ( 'NONE',  ( 235.3564303562499447, -32.72812499938547859, 99.99999999999998579 ) ) ;
#12441 = CARTESIAN_POINT ( 'NONE',  ( -85.15643035624999868, -32.01562499938548711, 101.5914258081833879 ) ) ;
#12442 = CARTESIAN_POINT ( 'NONE',  ( 235.3564303562499447, -33.62812499938547717, -50.00000000000011369 ) ) ;
#12443 = CARTESIAN_POINT ( 'NONE',  ( -82.39999999999999147, -31.68750000000000355, 103.4641016151377499 ) ) ;
#12444 = ORIENTED_EDGE ( 'NONE', *, *, #5654, .T. ) ;
#12445 = FACE_OUTER_BOUND ( 'NONE', #13778, .T. ) ;
#12446 = CARTESIAN_POINT ( 'NONE',  ( 96.99999999999994316, -29.80000000000000426, -150.0000000000000000 ) ) ;
#12447 = CARTESIAN_POINT ( 'NONE',  ( 79.64356964375001269, -33.02812499938548285, 101.5914258081833879 ) ) ;
#12448 = EDGE_CURVE ( 'NONE', #11379, #15250, #13541, .T. ) ;
#12449 = CARTESIAN_POINT ( 'NONE',  ( 84.56803305035325025, -32.00000000000000000, -101.7116913729796863 ) ) ;
#12450 = CARTESIAN_POINT ( 'NONE',  ( -82.39999999999999147, -32.61562499938548854, 96.81714838363319586 ) ) ;
#12451 = CARTESIAN_POINT ( 'NONE',  ( -85.15643035625001289, -32.50312499938548427, -99.99999999999998579 ) ) ;
#12452 = CARTESIAN_POINT ( 'NONE',  ( 85.15643035624999868, -30.17812499938548498, 101.5914258081833879 ) ) ;
#12453 = EDGE_CURVE ( 'NONE', #677, #5441, #2056, .T. ) ;
#12454 = CARTESIAN_POINT ( 'NONE',  ( 81.02178482187500208, -30.55312499938548854, -102.3871387122750889 ) ) ;
#12455 = FACE_OUTER_BOUND ( 'NONE', #11504, .T. ) ;
#12456 = CARTESIAN_POINT ( 'NONE',  ( -83.77821517812500929, -34.82812499938548711, 97.61286128772489690 ) ) ;
#12457 = CARTESIAN_POINT ( 'NONE',  ( -83.77821517812500929, -34.37812499938548427, -102.3871387122750889 ) ) ;
#12458 = ORIENTED_EDGE ( 'NONE', *, *, #9491, .T. ) ;
#12459 = CARTESIAN_POINT ( 'NONE',  ( 82.39999999999999147, -31.94062499938548427, 96.81714838363319586 ) ) ;
#12460 = CARTESIAN_POINT ( 'NONE',  ( -81.02178482187500208, -34.45312499938548711, 97.61286128772489690 ) ) ;
#12461 = CARTESIAN_POINT ( 'NONE',  ( 82.39999999999999147, -32.98124999877096286, 96.99999999999998579 ) ) ;
#12462 = ORIENTED_EDGE ( 'NONE', *, *, #187, .T. ) ;
#12463 = CARTESIAN_POINT ( 'NONE',  ( -80.90000000000000568, -32.85000000000000142, -102.5980762113533018 ) ) ;
#12464 = B_SPLINE_CURVE_WITH_KNOTS ( 'NONE', 3,
 ( #19159, #16130, #17692, #1285, #19065 ),
 .UNSPECIFIED., .F., .F.,
 ( 4, 1, 4 ),
 ( 5.640274452250024914E-20, 0.002309401076758505356, 0.004618802153517010713 ),
 .UNSPECIFIED. ) ;
#12465 = PRODUCT ( 'leg', 'leg', '', ( #15418 ) ) ;
#12466 = EDGE_CURVE ( 'NONE', #5913, #198, #1445, .T. ) ;
#12467 = CARTESIAN_POINT ( 'NONE',  ( 94.79999999999991189, -3.000000000000000000, -150.0000000000000000 ) ) ;
#12468 = CARTESIAN_POINT ( 'NONE',  ( -85.40000000000000568, -30.03749999999999787, 98.26794919243111792 ) ) ;
#12469 = CARTESIAN_POINT ( 'NONE',  ( -82.40000000000000568, -30.00000000000000355, 99.99999999999998579 ) ) ;
#12470 = ADVANCED_FACE ( 'NONE', ( #8794 ), #13097, .F. ) ;
#12471 = CARTESIAN_POINT ( 'NONE',  ( 233.9782151781249411, -34.90312499938547575, 97.61286128772489690 ) ) ;
#12472 = CARTESIAN_POINT ( 'NONE',  ( -82.39999999999999147, -35.01018749875868252, 96.53589838486223584 ) ) ;
#12473 = ORIENTED_EDGE ( 'NONE', *, *, #4755, .F. ) ;
#12474 = CARTESIAN_POINT ( 'NONE',  ( -82.39999999999999147, -34.86562499938548854, 96.81714838363319586 ) ) ;
#12475 = CARTESIAN_POINT ( 'NONE',  ( 83.20384757729338787, -34.59240381056766722, -97.00000000000000000 ) ) ;
#12476 = CARTESIAN_POINT ( 'NONE',  ( 230.3249173797030096, -31.99999999999999289, 101.5663513044663091 ) ) ;
#12477 = CARTESIAN_POINT ( 'NONE',  ( 82.40000000000000568, -34.38749999999999574, 96.99999999999998579 ) ) ;
#12478 = CARTESIAN_POINT ( 'NONE',  ( 244.7999999999999545, -29.80000000000002203, 153.0000000000000000 ) ) ;
#12479 = CARTESIAN_POINT ( 'NONE',  ( 85.15643035624999868, -30.74062499938548143, -98.40857419181659793 ) ) ;
#12480 = FACE_OUTER_BOUND ( 'NONE', #9603, .T. ) ;
#12481 = ORIENTED_EDGE ( 'NONE', *, *, #11374, .T. ) ;
#12482 = CARTESIAN_POINT ( 'NONE',  ( 83.90000000000000568, -30.91874999877096997, 102.5980762113533018 ) ) ;
#12483 = CARTESIAN_POINT ( 'NONE',  ( 233.9782151781249411, -31.75312499938547717, 97.61286128772489690 ) ) ;
#12484 = CARTESIAN_POINT ( 'NONE',  ( 231.2217848218749339, -31.07812499938548001, -47.61286128772501769 ) ) ;
#12485 = CARTESIAN_POINT ( 'NONE',  ( -82.39999999999999147, -32.27812499938548285, 103.1828516163667899 ) ) ;
#12486 = LINE ( 'NONE', #489, #18979 ) ;
#12487 = ORIENTED_EDGE ( 'NONE', *, *, #10001, .F. ) ;
#12488 = EDGE_LOOP ( 'NONE', ( #16955, #18267, #15615, #15643 ) ) ;
#12489 = CARTESIAN_POINT ( 'NONE',  ( -85.15643035624999868, -31.90312499938548285, -98.40857419181659793 ) ) ;
#12490 = CARTESIAN_POINT ( 'NONE',  ( -82.40000000000001990, -33.88124999877096855, -97.00000000000000000 ) ) ;
#12491 = LINE ( 'NONE', #11652, #6307 ) ;
#12492 = ORIENTED_EDGE ( 'NONE', *, *, #17037, .T. ) ;
#12493 = CARTESIAN_POINT ( 'NONE',  ( -82.39999999999999147, -31.40624999877096712, 96.99999999999998579 ) ) ;
#12494 = CARTESIAN_POINT ( 'NONE',  ( -83.90000000000000568, -33.46874999877096712, -97.40192378864668399 ) ) ;
#12495 = CARTESIAN_POINT ( 'NONE',  ( -79.39999999999999147, -33.86250000000000426, 101.7320508075688537 ) ) ;
#12496 = CARTESIAN_POINT ( 'NONE',  ( -85.40000000000000568, -31.29374999877096997, 99.99999999999998579 ) ) ;
#12497 = EDGE_CURVE ( 'NONE', #13993, #6484, #1384, .T. ) ;
#12498 = CARTESIAN_POINT ( 'NONE',  ( -82.39999999999999147, -33.88124999877096855, 103.4641016151377499 ) ) ;
#12499 = DIRECTION ( 'NONE',  ( 0.000000000000000000, 0.000000000000000000, 1.000000000000000000 ) ) ;
#12500 = CARTESIAN_POINT ( 'NONE',  ( 104.5000000000000142, 12.69999999999998508, 50.00000000000001421 ) ) ;
#12501 = CARTESIAN_POINT ( 'NONE',  ( 82.39999999999999147, -33.65624999877097423, -97.00000000000000000 ) ) ;
#12502 = CARTESIAN_POINT ( 'NONE',  ( 229.8435696437499871, -34.60312499938547859, 101.5914258081833879 ) ) ;
#12503 = EDGE_LOOP ( 'NONE', ( #14450, #15541, #12458, #9379, #10933 ) ) ;
#12504 = FILL_AREA_STYLE ('',( #2444 ) ) ;
#12505 = EDGE_CURVE ( 'NONE', #11141, #14672, #18877, .T. ) ;
#12506 = DIRECTION ( 'NONE',  ( -0.000000000000000000, -0.000000000000000000, -1.000000000000000000 ) ) ;
#12507 = PRODUCT_DEFINITION ( 'UNKNOWN', '', #15500, #4759 ) ;
#12508 = CARTESIAN_POINT ( 'NONE',  ( -80.90000000000000568, -32.94374999877096855, -97.40192378864668399 ) ) ;
#12509 = ORIENTED_EDGE ( 'NONE', *, *, #3784, .F. ) ;
#12510 = DIRECTION ( 'NONE',  ( -4.625929269271494788E-16, -1.000000000000000000, 0.000000000000000000 ) ) ;
#12511 = UNCERTAINTY_MEASURE_WITH_UNIT (LENGTH_MEASURE( 1.000000000000000082E-05 ), #15251, 'distance_accuracy_value', 'NONE');
#12512 = CARTESIAN_POINT ( 'NONE',  ( 4.000000000000000000, -2.309401076758516691, -0.4999999999999995559 ) ) ;
#12513 = ORIENTED_EDGE ( 'NONE', *, *, #13417, .T. ) ;
#12514 = CARTESIAN_POINT ( 'NONE',  ( 232.5999999999999375, -34.75312499938547717, -53.18285161636690361 ) ) ;
#12515 = CARTESIAN_POINT ( 'NONE',  ( 234.0999999999999375, -33.84374999877096002, -47.40192378864679768 ) ) ;
#12516 = VERTEX_POINT ( 'NONE', #15043 ) ;
#12517 = CARTESIAN_POINT ( 'NONE',  ( -82.40000000000001990, -31.18124999877096926, 103.0000000000000000 ) ) ;
#12518 = CARTESIAN_POINT ( 'NONE',  ( 85.40000000000000568, -30.48749999999999716, -98.26794919243111792 ) ) ;
#12519 = CARTESIAN_POINT ( 'NONE',  ( 4.050823680195225762, -3.779313952391384568, 0.5899027668435158356 ) ) ;
#12520 = CARTESIAN_POINT ( 'NONE',  ( -79.39999999999999147, -33.80624999877097281, 101.7320508075688537 ) ) ;
#12521 = CARTESIAN_POINT ( 'NONE',  ( -79.39999999999999147, -34.68356250001230023, 98.26794919243110371 ) ) ;
#12522 = CARTESIAN_POINT ( 'NONE',  ( 83.20384757729337366, -32.34240381056766722, -97.00000000000000000 ) ) ;
#12523 = LINE ( 'NONE', #19167, #15995 ) ;
#12524 = CARTESIAN_POINT ( 'NONE',  ( 85.15643035625001289, -33.85312499938549280, -99.99999999999998579 ) ) ;
#12525 = CARTESIAN_POINT ( 'NONE',  ( 4.071447262713887127, 2.020725942163686728, -3.499999999999999556 ) ) ;
#12526 = CARTESIAN_POINT ( 'NONE',  ( -82.39999999999999147, -34.07812499938548711, 103.1828516163667899 ) ) ;
#12527 = CARTESIAN_POINT ( 'NONE',  ( 82.39999999999999147, -32.95312499938548711, -96.81714838363319586 ) ) ;
#12528 = EDGE_LOOP ( 'NONE', ( #15498, #5589, #10038, #4959 ) ) ;
#12529 =( BOUNDED_CURVE ( )  B_SPLINE_CURVE ( 2, ( #1942, #18173, #493, #10641, #3215, #116, #13670, #14947, #10737 ),
 .UNSPECIFIED., .F., .F. ) 
 B_SPLINE_CURVE_WITH_KNOTS ( ( 3, 2, 2, 2, 3 ),
 ( 0.8541666666666665186, 0.8611111111111111605, 0.8750000000000000000, 0.8888888888888888395, 0.8958333333333333703 ),
 .UNSPECIFIED. ) 
 CURVE ( )  GEOMETRIC_REPRESENTATION_ITEM ( )  RATIONAL_B_SPLINE_CURVE ( ( 0.9330127018922194093, 0.9330127018922177440, 1.000000000000000000, 0.8660254037844387076, 1.000000000000000000, 0.8660254037844387076, 1.000000000000000000, 0.9330127018922187432, 0.9330127018922192983 ) ) 
 REPRESENTATION_ITEM ( '' )  );
#12530 = CARTESIAN_POINT ( 'NONE',  ( 235.3140393761304949, -32.00000000000000000, -48.72172371342785624 ) ) ;
#12531 = DIRECTION ( 'NONE',  ( 0.000000000000000000, 0.000000000000000000, 1.000000000000000000 ) ) ;
#12532 = CARTESIAN_POINT ( 'NONE',  ( -83.20384757729335945, -33.90134618820329848, 102.9999999999999716 ) ) ;
#12533 = CARTESIAN_POINT ( 'NONE',  ( 229.8435696437499587, -32.46562499938548285, 101.5914258081833879 ) ) ;
#12534 = CARTESIAN_POINT ( 'NONE',  ( -81.02178482187500208, -31.45312499938549067, 102.3871387122750889 ) ) ;
#12535 = CARTESIAN_POINT ( 'NONE',  ( 229.8435696437499303, -32.05312499938548143, -50.00000000000011369 ) ) ;
#12536 = CARTESIAN_POINT ( 'NONE',  ( -85.40000000000000568, -31.83750000000000568, 98.26794919243111792 ) ) ;
#12537 = EDGE_LOOP ( 'NONE', ( #8768, #13715, #4421, #3856 ) ) ;
#12538 = CARTESIAN_POINT ( 'NONE',  ( 0.02993401039713562001, 2.688325911136453250, -2.343682934607766111 ) ) ;
#12539 = CARTESIAN_POINT ( 'NONE',  ( -79.39999999999999147, -34.70624999877097139, 101.7320508075688537 ) ) ;
#12540 = CARTESIAN_POINT ( 'NONE',  ( 85.15643035624999868, -31.52812499938547930, 101.5914258081833879 ) ) ;
#12541 = VECTOR ( 'NONE', #2736, 1000.000000000000000 ) ;
#12542 = AXIS2_PLACEMENT_3D ( 'NONE', #18083, #1753, #400 ) ;
#12543 = CARTESIAN_POINT ( 'NONE',  ( 85.03799702444355546, -31.99999999999997868, -99.18121545504337178 ) ) ;
#12544 = CARTESIAN_POINT ( 'NONE',  ( -82.39999999999999147, -31.49062499938548143, 103.1828516163667899 ) ) ;
#12545 = CARTESIAN_POINT ( 'NONE',  ( -79.64356964374999848, -32.72812499938548569, -99.99999999999998579 ) ) ;
#12546 = CARTESIAN_POINT ( 'NONE',  ( 82.39999999999999147, -33.40312499938548285, 103.1828516163667899 ) ) ;
#12547 = CARTESIAN_POINT ( 'NONE',  ( 81.02178482187500208, -32.80312499938548854, -102.3871387122750889 ) ) ;
#12548 = CARTESIAN_POINT ( 'NONE',  ( 233.9782151781249411, -30.74062499938547788, -52.38713871227520968 ) ) ;
#12549 = CARTESIAN_POINT ( 'NONE',  ( -81.02178482187500208, -34.60312499938549280, 102.3871387122750889 ) ) ;
#12550 = CARTESIAN_POINT ( 'NONE',  ( -83.77821517812500929, -34.22812499938549280, -97.61286128772489690 ) ) ;
#12551 = ORIENTED_EDGE ( 'NONE', *, *, #6395, .F. ) ;
#12552 = CARTESIAN_POINT ( 'NONE',  ( 85.15643035624999868, -32.91562499938549280, 98.40857419181659793 ) ) ;
#12553 = DIRECTION ( 'NONE',  ( 0.3420201433256622736, 1.150791560227853228E-16, 0.9396926207859106484 ) ) ;
#12554 = VECTOR ( 'NONE', #16903, 1000.000000000000000 ) ;
#12555 = CARTESIAN_POINT ( 'NONE',  ( -81.02178482187500208, -31.79062499938548925, 102.3871387122750889 ) ) ;
#12556 = AXIS2_PLACEMENT_3D ( 'NONE', #11330, #8395, #11035 ) ;
#12557 = CARTESIAN_POINT ( 'NONE',  ( -79.64356964374999848, -33.17812499938548854, 99.99999999999998579 ) ) ;
#12558 = CARTESIAN_POINT ( 'NONE',  ( -83.90000000000000568, -31.27500000000000568, 102.5980762113533018 ) ) ;
#12559 = VERTEX_POINT ( 'NONE', #12207 ) ;
#12560 = CARTESIAN_POINT ( 'NONE',  ( -79.39999999999999147, -34.27499999999999858, -99.99999999999998579 ) ) ;
#12561 = ADVANCED_FACE ( 'NONE', ( #3027 ), #1853, .F. ) ;
#12562 = ADVANCED_FACE ( 'NONE', ( #16704 ), #13673, .T. ) ;
#12563 = CARTESIAN_POINT ( 'NONE',  ( 79.39999999999999147, -32.96250000000000568, -101.7320508075688537 ) ) ;
#12564 = CARTESIAN_POINT ( 'NONE',  ( 229.5999999999999375, -34.01249999999999574, -48.26794919243123161 ) ) ;
#12565 = CARTESIAN_POINT ( 'NONE',  ( -85.15643035624999868, -34.71562499938548285, -98.40857419181659793 ) ) ;
#12566 = CARTESIAN_POINT ( 'NONE',  ( 232.5999999999999375, -33.96562499938547575, 96.81714838363319586 ) ) ;
#12567 = CARTESIAN_POINT ( 'NONE',  ( -85.40000000000000568, -33.54768749875866973, 99.99999999999998579 ) ) ;
#12568 = VERTEX_POINT ( 'NONE', #14950 ) ;
#12569 = CARTESIAN_POINT ( 'NONE',  ( 231.0999999999999375, -32.77499999999999147, 97.40192378864668399 ) ) ;
#12570 = CARTESIAN_POINT ( 'NONE',  ( 85.40000000000000568, -34.46249999999999858, -101.7320508075688821 ) ) ;
#12571 = CARTESIAN_POINT ( 'NONE',  ( -83.90000000000000568, -33.46874999877096712, -97.40192378864668399 ) ) ;
#12572 = DIRECTION ( 'NONE',  ( -0.000000000000000000, -0.000000000000000000, -1.000000000000000000 ) ) ;
#12573 = AXIS2_PLACEMENT_3D ( 'NONE', #8817, #5899, #10476 ) ;
#12574 = LINE ( 'NONE', #7794, #12392 ) ;
#12575 = CARTESIAN_POINT ( 'NONE',  ( 85.15643035624999868, -31.19062499938548783, -98.40857419181659793 ) ) ;
#12576 = CARTESIAN_POINT ( 'NONE',  ( 230.2961164517930968, -35.00002705695767702, -51.92148140967023551 ) ) ;
#12577 = EDGE_CURVE ( 'NONE', #2207, #4201, #9229, .T. ) ;
#12578 = ORIENTED_EDGE ( 'NONE', *, *, #6183, .F. ) ;
#12579 = CARTESIAN_POINT ( 'NONE',  ( 85.40000000000000568, -31.70624999877096784, 98.26794919243111792 ) ) ;
#12580 = SHAPE_DEFINITION_REPRESENTATION ( #18730, #14995 ) ;
#12581 = CARTESIAN_POINT ( 'NONE',  ( 233.9782151781249411, -32.35312499938547859, 102.3871387122750889 ) ) ;
#12582 = CARTESIAN_POINT ( 'NONE',  ( 232.5999999999999375, -33.74062499938548143, -46.81714838363331666 ) ) ;
#12583 = CARTESIAN_POINT ( 'NONE',  ( -85.15643035625001289, -34.64062499938548711, 99.99999999999998579 ) ) ;
#12584 = CARTESIAN_POINT ( 'NONE',  ( 82.40000000000000568, -34.10624999877096997, 102.9999999999999858 ) ) ;
#12585 = ORIENTED_EDGE ( 'NONE', *, *, #7168, .T. ) ;
#12586 = EDGE_LOOP ( 'NONE', ( #16604, #8495, #16922, #18557 ) ) ;
#12587 = CARTESIAN_POINT ( 'NONE',  ( -85.15643035624999868, -31.00312499938548072, -98.40857419181659793 ) ) ;
#12588 = EDGE_CURVE ( 'NONE', #5276, #11697, #10359, .T. ) ;
#12589 = ORIENTED_EDGE ( 'NONE', *, *, #14382, .F. ) ;
#12590 = CARTESIAN_POINT ( 'NONE',  ( 83.77821517812500929, -33.02812499938548285, 102.3871387122750889 ) ) ;
#12591 = CARTESIAN_POINT ( 'NONE',  ( -80.90000000000000568, -34.74374999877097281, -97.40192378864668399 ) ) ;
#12592 = CARTESIAN_POINT ( 'NONE',  ( 79.39999999999999147, -33.37500000000000000, 99.99999999999998579 ) ) ;
#12593 = CARTESIAN_POINT ( 'NONE',  ( -81.59615242270663771, -32.11740381056766580, 103.0000000000000000 ) ) ;
#12594 = CARTESIAN_POINT ( 'NONE',  ( -85.40000000000000568, -31.78124999877096712, 98.26794919243111792 ) ) ;
#12595 = CARTESIAN_POINT ( 'NONE',  ( -80.90000000000000568, -32.94374999877096855, 102.5980762113533018 ) ) ;
#12596 = CYLINDRICAL_SURFACE ( 'NONE', #9137, 3.000000000000002665 ) ;
#12597 =( BOUNDED_CURVE ( )  B_SPLINE_CURVE ( 2, ( #3734, #17513, #12917, #1095, #9699, #3929, #12822, #2465, #18787 ),
 .UNSPECIFIED., .F., .F. ) 
 B_SPLINE_CURVE_WITH_KNOTS ( ( 3, 2, 2, 2, 3 ),
 ( 0.1875000000000000000, 0.1944444444444444475, 0.2083333333333333426, 0.2222222222222222099, 0.2291666666666666297 ),
 .UNSPECIFIED. ) 
 CURVE ( )  GEOMETRIC_REPRESENTATION_ITEM ( )  RATIONAL_B_SPLINE_CURVE ( ( 0.9330127018922194093, 0.9330127018922194093, 1.000000000000000000, 0.8660254037844387076, 1.000000000000000000, 0.8660254037844387076, 1.000000000000000000, 0.9330127018922196314, 0.9330127018922194093 ) ) 
 REPRESENTATION_ITEM ( '' )  );
#12598 = CARTESIAN_POINT ( 'NONE',  ( 79.39999999999999147, -34.25624999877096855, -101.7320508075688537 ) ) ;
#12599 = DIRECTION ( 'NONE',  ( -0.000000000000000000, -1.000000000000000000, 3.597944987211154374E-15 ) ) ;
#12600 = CARTESIAN_POINT ( 'NONE',  ( 232.5999999999999375, -34.07812499938548001, 103.1828516163667899 ) ) ;
#12601 = ORIENTED_EDGE ( 'NONE', *, *, #14734, .F. ) ;
#12602 = CARTESIAN_POINT ( 'NONE',  ( 81.02178482187500208, -32.09062499938548285, -97.61286128772489690 ) ) ;
#12603 = CARTESIAN_POINT ( 'NONE',  ( 229.5999999999999375, -31.33124999877096073, 98.26794919243111792 ) ) ;
#12604 = FACE_OUTER_BOUND ( 'NONE', #7680, .T. ) ;
#12605 = EDGE_LOOP ( 'NONE', ( #9895, #16823, #15997, #7164 ) ) ;
#12606 = DIRECTION ( 'NONE',  ( 0.000000000000000000, -1.000000000000000000, 0.000000000000000000 ) ) ;
#12607 = CARTESIAN_POINT ( 'NONE',  ( 111.5000000000000142, 12.69999999999998508, 110.0000000000000142 ) ) ;
#12608 = FACE_OUTER_BOUND ( 'NONE', #3743, .T. ) ;
#12609 = ORIENTED_EDGE ( 'NONE', *, *, #4040, .F. ) ;
#12610 = CARTESIAN_POINT ( 'NONE',  ( 3.880206590543342493, -3.396506438958446061, 1.117078279489142512 ) ) ;
#12611 = CARTESIAN_POINT ( 'NONE',  ( 4.154306624730763176, -2.398490048084970461, -3.721999068284303824 ) ) ;
#12612 = EDGE_LOOP ( 'NONE', ( #14306, #4111, #13181, #6610 ) ) ;
#12613 = CARTESIAN_POINT ( 'NONE',  ( -81.59615242270663771, -32.11740381056766580, -96.99999999999998579 ) ) ;
#12614 = CARTESIAN_POINT ( 'NONE',  ( 82.39999999999999147, -30.56250000000000355, -96.53589838486223584 ) ) ;
#12615 = CARTESIAN_POINT ( 'NONE',  ( -79.77811200999879304, -35.00000000000000000, -99.14934632385212865 ) ) ;
#12616 = CARTESIAN_POINT ( 'NONE',  ( -85.40000000000000568, -34.48124999877096997, 98.26794919243111792 ) ) ;
#12617 = CARTESIAN_POINT ( 'NONE',  ( -85.40000000000000568, -34.04606250001229739, 99.99999999999998579 ) ) ;
#12618 = EDGE_CURVE ( 'NONE', #3019, #1356, #4498, .T. ) ;
#12619 = CARTESIAN_POINT ( 'NONE',  ( 82.39999999999999147, -32.36250000000000426, -96.99999999999997158 ) ) ;
#12620 = CARTESIAN_POINT ( 'NONE',  ( 0.2182387239031244319, 1.693823289467349724, -3.499999999999999556 ) ) ;
#12621 = CARTESIAN_POINT ( 'NONE',  ( 229.5999999999999375, -32.15624999877096002, -48.26794919243123161 ) ) ;
#12622 = CARTESIAN_POINT ( 'NONE',  ( -82.39999999999999147, -33.48750000000000426, 103.0000000000000000 ) ) ;
#12623 = CARTESIAN_POINT ( 'NONE',  ( -79.64356964374999848, -33.96562499938548285, 99.99999999999998579 ) ) ;
#12624 = DIRECTION ( 'NONE',  ( -1.000000000000000000, 0.000000000000000000, 0.000000000000000000 ) ) ;
#12625 = ORIENTED_EDGE ( 'NONE', *, *, #18550, .T. ) ;
#12626 = CARTESIAN_POINT ( 'NONE',  ( 234.0999999999999375, -34.64999999999999147, -52.59807621135342970 ) ) ;
#12627 = CARTESIAN_POINT ( 'NONE',  ( -80.90000000000000568, -34.20000000000000284, 97.40192378864668399 ) ) ;
#12628 = PRODUCT_DEFINITION_SHAPE ( 'NONE', 'NONE',  #19335 ) ;
#12629 = CARTESIAN_POINT ( 'NONE',  ( -85.40000000000000568, -33.95624999877097139, 101.7320508075688821 ) ) ;
#12630 = CARTESIAN_POINT ( 'NONE',  ( 82.40000000000000568, -33.71249999999998437, 102.9999999999999858 ) ) ;
#12631 = CARTESIAN_POINT ( 'NONE',  ( -85.15643035625001289, -34.75312499938548427, 99.99999999999998579 ) ) ;
#12632 = CARTESIAN_POINT ( 'NONE',  ( 229.8435696437499871, -31.45312499938547290, -48.40857419181671162 ) ) ;
#12633 = ORIENTED_EDGE ( 'NONE', *, *, #13046, .T. ) ;
#12634 = CARTESIAN_POINT ( 'NONE',  ( 0.000000000000000000, 3.031088913245532979, -1.750000000000004219 ) ) ;
#12635 = CARTESIAN_POINT ( 'NONE',  ( -81.59615242270662350, -33.73259618943233562, -102.9999999999999858 ) ) ;
#12636 = CARTESIAN_POINT ( 'NONE',  ( 85.15643035624999868, -32.42812499938548854, 101.5914258081833879 ) ) ;
#12637=STYLED_ITEM('',(#19378),#9400);
#12638 = CARTESIAN_POINT ( 'NONE',  ( 79.39999999999999147, -32.02500000000000568, -99.99999999999998579 ) ) ;
#12639 =( BOUNDED_CURVE ( )  B_SPLINE_CURVE ( 2, ( #7343, #8711, #16532, #6082, #14861, #13296, #18101, #16624, #1299 ),
 .UNSPECIFIED., .F., .F. ) 
 B_SPLINE_CURVE_WITH_KNOTS ( ( 3, 2, 2, 2, 3 ),
 ( 0.4374999999999999445, 0.4444444444444444198, 0.4583333333333333148, 0.4722222222222222099, 0.4791666666666665186 ),
 .UNSPECIFIED. ) 
 CURVE ( )  GEOMETRIC_REPRESENTATION_ITEM ( )  RATIONAL_B_SPLINE_CURVE ( ( 0.9330127018922192983, 0.9330127018922187432, 1.000000000000000000, 0.8660254037844387076, 1.000000000000000000, 0.8660254037844387076, 1.000000000000000000, 0.9330127018922207416, 0.9330127018922194093 ) ) 
 REPRESENTATION_ITEM ( '' )  );
#12640 = CARTESIAN_POINT ( 'NONE',  ( -82.39999999999999147, -33.29062499938548569, 103.1828516163667899 ) ) ;
#12641 = CARTESIAN_POINT ( 'NONE',  ( 82.86160995759657055, -31.99999999999997158, 97.18959324165044222 ) ) ;
#12642 = CARTESIAN_POINT ( 'NONE',  ( 82.39999999999999147, -31.37812499938548427, 96.81714838363319586 ) ) ;
#12643 = CARTESIAN_POINT ( 'NONE',  ( 85.15643035624999868, -33.89062499938548711, -98.40857419181659793 ) ) ;
#12644 = CARTESIAN_POINT ( 'NONE',  ( 229.8435696437499871, -32.35312499938547859, -48.40857419181671162 ) ) ;
#12645 = CARTESIAN_POINT ( 'NONE',  ( -82.39999999999999147, -33.06562499938548427, 96.81714838363319586 ) ) ;
#12646 = CARTESIAN_POINT ( 'NONE',  ( -79.64356964374999848, -31.71562499938548285, -99.99999999999998579 ) ) ;
#12647 = ORIENTED_EDGE ( 'NONE', *, *, #18735, .T. ) ;
#12648 = CARTESIAN_POINT ( 'NONE',  ( 79.64356964375001269, -32.76562499938548711, 98.40857419181659793 ) ) ;
#12649 = ADVANCED_FACE ( 'NONE', ( #15139, #1575, #1756 ), #16611, .F. ) ;
#12650 = CARTESIAN_POINT ( 'NONE',  ( -85.40000000000000568, -33.09374999877096712, 99.99999999999998579 ) ) ;
#12651 = CARTESIAN_POINT ( 'NONE',  ( -83.90000000000000568, -34.12500000000000000, 97.40192378864668399 ) ) ;
#12652 = VECTOR ( 'NONE', #17548, 1000.000000000000000 ) ;
#12653 = CARTESIAN_POINT ( 'NONE',  ( -79.64356964374999848, -31.26562499938548356, 99.99999999999998579 ) ) ;
#12654 = CARTESIAN_POINT ( 'NONE',  ( -79.64356964375001269, -33.66562499938549280, 101.5914258081833879 ) ) ;
#12655 = DIRECTION ( 'NONE',  ( 0.000000000000000000, 0.000000000000000000, 1.000000000000000000 ) ) ;
#12656 = EDGE_LOOP ( 'NONE', ( #16488, #17083, #4135, #17222 ) ) ;
#12657 = CARTESIAN_POINT ( 'NONE',  ( -83.90000000000000568, -32.77499999999999858, -102.5980762113533018 ) ) ;
#12658 = CARTESIAN_POINT ( 'NONE',  ( 230.5724978686189672, -35.00000000000000711, -52.22004150442379711 ) ) ;
#12659 = CARTESIAN_POINT ( 'NONE',  ( -82.39999999999999147, -32.98124999877096286, 102.9999999999999858 ) ) ;
#12660 = CARTESIAN_POINT ( 'NONE',  ( 229.8435696437499871, -32.42812499938548143, 98.40857419181659793 ) ) ;
#12661 = CARTESIAN_POINT ( 'NONE',  ( -80.90000000000000568, -33.84768749875867400, 102.5980762113533018 ) ) ;
#12662 = CARTESIAN_POINT ( 'NONE',  ( 82.40000000000000568, -30.00000000000000355, 103.0000000000000000 ) ) ;
#12663 = LINE ( 'NONE', #18636, #3618 ) ;
#12664 = CARTESIAN_POINT ( 'NONE',  ( 85.15643035624999868, -31.19062499938548783, 101.5914258081833879 ) ) ;
#12665 = VECTOR ( 'NONE', #12013, 1000.000000000000000 ) ;
#12666 = CARTESIAN_POINT ( 'NONE',  ( 105.5000000000000142, 12.69999999999998508, 110.0000000000000142 ) ) ;
#12667 = CARTESIAN_POINT ( 'NONE',  ( 4.071447262713887127, 2.020725942163688504, 3.500000000000000000 ) ) ;
#12668 = CARTESIAN_POINT ( 'NONE',  ( 85.15643035624999868, -32.01562499938548711, -101.5914258081833879 ) ) ;
#12669 = DIRECTION ( 'NONE',  ( 0.000000000000000000, 1.000000000000000000, 0.000000000000000000 ) ) ;
#12670 =( BOUNDED_CURVE ( )  B_SPLINE_CURVE ( 2, ( #11095, #3679, #16874, #2014, #8173, #9644, #15605, #6713, #12659 ),
 .UNSPECIFIED., .F., .F. ) 
 B_SPLINE_CURVE_WITH_KNOTS ( ( 3, 2, 2, 2, 3 ),
 ( 0.4374999999999999445, 0.4444444444444444198, 0.4583333333333333148, 0.4722222222222222099, 0.4791666666666666297 ),
 .UNSPECIFIED. ) 
 CURVE ( )  GEOMETRIC_REPRESENTATION_ITEM ( )  RATIONAL_B_SPLINE_CURVE ( ( 0.9330127018922192983, 0.9330127018922187432, 1.000000000000000000, 0.8660254037844387076, 1.000000000000000000, 0.8660254037844387076, 1.000000000000000000, 0.9330127018922196314, 0.9330127018922194093 ) ) 
 REPRESENTATION_ITEM ( '' )  );
#12671 = VERTEX_POINT ( 'NONE', #17987 ) ;
#12672 = CARTESIAN_POINT ( 'NONE',  ( 83.90000000000000568, -31.36874999877096926, 102.5980762113533018 ) ) ;
#12673 = PRODUCT_CONTEXT ( 'NONE', #94, 'mechanical' ) ;
#12674 = CARTESIAN_POINT ( 'NONE',  ( 229.8435696437499871, -32.46562499938548285, 101.5914258081833879 ) ) ;
#12675 = CARTESIAN_POINT ( 'NONE',  ( 235.3564303562499447, -33.62812499938547717, -50.00000000000011369 ) ) ;
#12676 = AXIS2_PLACEMENT_3D ( 'NONE', #12195, #7799, #10544 ) ;
#12677 = CARTESIAN_POINT ( 'NONE',  ( -85.15643035624999868, -33.25312499938548427, 101.5914258081833879 ) ) ;
#12678 = CARTESIAN_POINT ( 'NONE',  ( 231.0999999999999375, -32.77499999999999147, -52.59807621135342970 ) ) ;
#12679 = ORIENTED_EDGE ( 'NONE', *, *, #7571, .F. ) ;
#12680 = ORIENTED_EDGE ( 'NONE', *, *, #15182, .T. ) ;
#12681 = CARTESIAN_POINT ( 'NONE',  ( -81.02178482187500208, -32.24062499938548854, -97.61286128772489690 ) ) ;
#12682 = CARTESIAN_POINT ( 'NONE',  ( -94.79999999999999716, -35.00000000000000000, -150.0000000000000000 ) ) ;
#12683 = EDGE_LOOP ( 'NONE', ( #16226, #1254, #7852, #16074 ) ) ;
#12684 = EDGE_CURVE ( 'NONE', #7898, #1498, #8560, .T. ) ;
#12685 = CARTESIAN_POINT ( 'NONE',  ( 85.15643035625001289, -33.85312499938549280, 99.99999999999998579 ) ) ;
#12686 = CARTESIAN_POINT ( 'NONE',  ( -83.90000000000000568, -34.81874999877096855, -97.40192378864668399 ) ) ;
#12687 = EDGE_CURVE ( 'NONE', #1971, #5593, #10644, .T. ) ;
#12688 = FACE_OUTER_BOUND ( 'NONE', #10709, .T. ) ;
#12689 = CARTESIAN_POINT ( 'NONE',  ( -79.77811200999887831, -35.00000000000000000, 100.8506536761481414 ) ) ;
#12690 = CARTESIAN_POINT ( 'NONE',  ( -79.39999999999999147, -33.28124999877096712, 98.26794919243110371 ) ) ;
#12691 = CARTESIAN_POINT ( 'NONE',  ( -85.40000000000000568, -34.44374999877096855, 99.99999999999998579 ) ) ;
#12692 = CARTESIAN_POINT ( 'NONE',  ( 85.29357727955090240, -35.00000000000000000, -100.3154961327749817 ) ) ;
#12693 = CARTESIAN_POINT ( 'NONE',  ( 231.5800379434388674, -35.00000000000000000, 97.17173842519744653 ) ) ;
#12694 = CARTESIAN_POINT ( 'NONE',  ( -82.40000000000000568, -33.71249999999998437, 96.99999999999998579 ) ) ;
#12695 = VECTOR ( 'NONE', #13463, 1000.000000000000000 ) ;
#12696 = CARTESIAN_POINT ( 'NONE',  ( 235.3564303562499447, -34.90312499938547575, 101.5914258081833879 ) ) ;
#12697 = EDGE_CURVE ( 'NONE', #4279, #9797, #18690, .T. ) ;
#12698 = ORIENTED_EDGE ( 'NONE', *, *, #14007, .T. ) ;
#12699 = CARTESIAN_POINT ( 'NONE',  ( 82.39999999999999147, -33.85312499938548569, -96.81714838363319586 ) ) ;
#12700 = FACE_OUTER_BOUND ( 'NONE', #5772, .T. ) ;
#12701 = CARTESIAN_POINT ( 'NONE',  ( 231.0999999999999375, -31.66874999877096641, -47.40192378864679768 ) ) ;
#12702 = VERTEX_POINT ( 'NONE', #9270 ) ;
#12703 = CARTESIAN_POINT ( 'NONE',  ( 232.5999999999999375, -34.61249999999999716, 97.00000000000000000 ) ) ;
#12704 = CARTESIAN_POINT ( 'NONE',  ( -81.02178482187500208, -31.34062499938548996, 102.3871387122750889 ) ) ;
#12705 = AXIS2_PLACEMENT_3D ( 'NONE', #17106, #3717, #9682 ) ;
#12706 = CARTESIAN_POINT ( 'NONE',  ( 0.000000000000000000, 0.000000000000000000, 3.469446951953614189E-15 ) ) ;
#12707 = ORIENTED_EDGE ( 'NONE', *, *, #9854, .F. ) ;
#12708 = B_SPLINE_CURVE_WITH_KNOTS ( 'NONE', 3,
 ( #13280, #19157, #8884, #5592, #2835, #19062 ),
 .UNSPECIFIED., .F., .F.,
 ( 4, 2, 4 ),
 ( 0.002452478801916361129, 0.003676905084148001344, 0.004901331366379641126 ),
 .UNSPECIFIED. ) ;
#12709 = CARTESIAN_POINT ( 'NONE',  ( 4.055492966679648426, -3.795017426214730705, 0.5629142681441111629 ) ) ;
#12710 = CARTESIAN_POINT ( 'NONE',  ( 229.5999999999999375, -33.09374999877096002, 99.99999999999998579 ) ) ;
#12711 = EDGE_LOOP ( 'NONE', ( #15599, #1096, #16031, #1993 ) ) ;
#12712 = LINE ( 'NONE', #17406, #5160 ) ;
#12713 = EDGE_CURVE ( 'NONE', #17759, #3211, #19308, .T. ) ;
#12714 = CARTESIAN_POINT ( 'NONE',  ( 80.90000000000000568, -33.89999999999999858, -102.5980762113533018 ) ) ;
#12715 = DIRECTION ( 'NONE',  ( -0.000000000000000000, -1.000000000000000000, -0.000000000000000000 ) ) ;
#12716 = VECTOR ( 'NONE', #9351, 1000.000000000000000 ) ;
#12717 =( BOUNDED_CURVE ( )  B_SPLINE_CURVE ( 2, ( #2306, #5455, #9935, #16084, #14504, #15892, #858, #2690, #1049 ),
 .UNSPECIFIED., .F., .F. ) 
 B_SPLINE_CURVE_WITH_KNOTS ( ( 3, 2, 2, 2, 3 ),
 ( 0.4374999999999999445, 0.4444444444444444198, 0.4583333333333333148, 0.4722222222222222099, 0.4791666666666666297 ),
 .UNSPECIFIED. ) 
 CURVE ( )  GEOMETRIC_REPRESENTATION_ITEM ( )  RATIONAL_B_SPLINE_CURVE ( ( 0.9330127018922192983, 0.9330127018922187432, 1.000000000000000000, 0.8660254037844387076, 1.000000000000000000, 0.8660254037844387076, 1.000000000000000000, 0.9330127018922196314, 0.9330127018922194093 ) ) 
 REPRESENTATION_ITEM ( '' )  );
#12718 = ADVANCED_FACE ( 'NONE', ( #14846 ), #1472, .F. ) ;
#12719 = CARTESIAN_POINT ( 'NONE',  ( -82.39999999999999147, -35.23124999877096997, 103.4641016151377499 ) ) ;
#12720 = CARTESIAN_POINT ( 'NONE',  ( -80.90000000000000568, -34.64606250001229171, 97.40192378864668399 ) ) ;
#12721 = LINE ( 'NONE', #9791, #13047 ) ;
#12722 = CARTESIAN_POINT ( 'NONE',  ( 81.59615242270662350, -33.41115380933863577, 96.99999999999998579 ) ) ;
#12723 = EDGE_CURVE ( 'NONE', #15743, #5107, #1888, .T. ) ;
#12724 = CARTESIAN_POINT ( 'NONE',  ( 82.40000000000000568, -34.38749999999999574, 96.99999999999998579 ) ) ;
#12725 = CIRCLE ( 'NONE', #6480, 2.649999999999982148 ) ;
#12726 = CARTESIAN_POINT ( 'NONE',  ( 3.951447005078448260, 1.347150628109122561, -3.499999999999999112 ) ) ;
#12727 = CARTESIAN_POINT ( 'NONE',  ( -79.64356964375001269, -33.47812499938547859, 98.40857419181659793 ) ) ;
#12728 = CARTESIAN_POINT ( 'NONE',  ( -96.99999999999998579, 0.000000000000000000, 150.0000000000000000 ) ) ;
#12729 = ORIENTED_EDGE ( 'NONE', *, *, #7932, .T. ) ;
#12730 = CARTESIAN_POINT ( 'NONE',  ( 231.0999999999999375, -34.12499999999999289, -52.59807621135342970 ) ) ;
#12731 = CARTESIAN_POINT ( 'NONE',  ( 235.5999999999999943, -33.28124999877096002, -51.73205080756900287 ) ) ;
#12732 = AXIS2_PLACEMENT_3D ( 'NONE', #10563, #9281, #10749 ) ;
#12733 = VECTOR ( 'NONE', #12382, 1000.000000000000000 ) ;
#12734 = CARTESIAN_POINT ( 'NONE',  ( 233.9782151781249411, -33.10312499938547859, 97.61286128772489690 ) ) ;
#12735 = CARTESIAN_POINT ( 'NONE',  ( -83.77821517812500929, -34.22812499938549280, 102.3871387122750889 ) ) ;
#12736 = EDGE_CURVE ( 'NONE', #9023, #9588, #5952, .T. ) ;
#12737 = CARTESIAN_POINT ( 'NONE',  ( 235.3564303562499447, -34.49062499938548143, -51.59142580818350865 ) ) ;
#12738 = ORIENTED_EDGE ( 'NONE', *, *, #16994, .T. ) ;
#12739 = CARTESIAN_POINT ( 'NONE',  ( -83.03192786677300319, -34.99999999999999289, -97.31096265645996368 ) ) ;
#12740 = CARTESIAN_POINT ( 'NONE',  ( -83.77821517812500929, -34.71562499938548285, 97.61286128772489690 ) ) ;
#12741 = CARTESIAN_POINT ( 'NONE',  ( -80.90000000000000568, -34.59374999877096712, 97.40192378864668399 ) ) ;
#12742 = CARTESIAN_POINT ( 'NONE',  ( 85.15643035624999868, -32.80312499938548854, 98.40857419181659793 ) ) ;
#12743 = CARTESIAN_POINT ( 'NONE',  ( 229.5999999999999375, -33.09374999877096002, -50.00000000000011369 ) ) ;
#12744 = CARTESIAN_POINT ( 'NONE',  ( 235.3564303562499447, -32.65312499938547575, -48.40857419181671162 ) ) ;
#12745 = EDGE_CURVE ( 'NONE', #14591, #17401, #8862, .T. ) ;
#12746 = CARTESIAN_POINT ( 'NONE',  ( -79.64356964374998427, -33.14062499938548711, 98.40857419181659793 ) ) ;
#12747 = CARTESIAN_POINT ( 'NONE',  ( -79.64356964374998427, -33.21562499938548996, -98.40857419181659793 ) ) ;
#12748 = CARTESIAN_POINT ( 'NONE',  ( 79.64356964374999848, -33.06562499938548427, 99.99999999999998579 ) ) ;
#12749 = CARTESIAN_POINT ( 'NONE',  ( 83.77821517812500929, -33.92812499938548854, -97.61286128772489690 ) ) ;
#12750 = CARTESIAN_POINT ( 'NONE',  ( 235.3564303562499447, -33.47812499938547148, -51.59142580818350865 ) ) ;
#12751 = CARTESIAN_POINT ( 'NONE',  ( -82.39999999999999147, -32.95312499938548711, 96.81714838363319586 ) ) ;
#12752 = ORIENTED_EDGE ( 'NONE', *, *, #555, .F. ) ;
#12753 = CARTESIAN_POINT ( 'NONE',  ( 81.02178482187500208, -31.75312499938548427, 102.3871387122750889 ) ) ;
#12754 = CARTESIAN_POINT ( 'NONE',  ( 235.5999999999999943, -34.25624999877096144, -48.26794919243124582 ) ) ;
#12755 = CARTESIAN_POINT ( 'NONE',  ( -85.40000000000000568, -34.05000000000000426, 99.99999999999998579 ) ) ;
#12756 = CARTESIAN_POINT ( 'NONE',  ( -85.15643035624999868, -30.17812499938548498, 98.40857419181659793 ) ) ;
#12757 = CARTESIAN_POINT ( 'NONE',  ( -85.15643035624999868, -31.97812499938548925, 98.40857419181659793 ) ) ;
#12758 = DIRECTION ( 'NONE',  ( -0.000000000000000000, -0.000000000000000000, 1.000000000000000000 ) ) ;
#12759 = ORIENTED_EDGE ( 'NONE', *, *, #18852, .F. ) ;
#12760 = B_SPLINE_CURVE_WITH_KNOTS ( 'NONE', 3,
 ( #16584, #6328, #13190, #19160, #3188, #15301 ),
 .UNSPECIFIED., .F., .F.,
 ( 4, 2, 4 ),
 ( 1.316110421120630972E-19, 0.002086519881787259317, 0.004173039763574518633 ),
 .UNSPECIFIED. ) ;
#12761 = CARTESIAN_POINT ( 'NONE',  ( -83.90000000000000568, -33.97500000000000853, -97.40192378864668399 ) ) ;
#12762 = DIRECTION ( 'NONE',  ( -0.000000000000000000, 1.000000000000000000, 0.000000000000000000 ) ) ;
#12763 = CARTESIAN_POINT ( 'NONE',  ( -83.90000000000000568, -30.07499999999999929, 97.40192378864668399 ) ) ;
#12764 = CARTESIAN_POINT ( 'NONE',  ( -83.90000000000000568, -30.07106250001229242, 97.40192378864668399 ) ) ;
#12765 = DIRECTION ( 'NONE',  ( -0.000000000000000000, -1.000000000000000000, -0.000000000000000000 ) ) ;
#12766 = DIRECTION ( 'NONE',  ( 0.000000000000000000, 0.000000000000000000, 1.000000000000000000 ) ) ;
#12767 = DIRECTION ( 'NONE',  ( 0.000000000000000000, 0.000000000000000000, 1.000000000000000000 ) ) ;
#12768 = CARTESIAN_POINT ( 'NONE',  ( 230.4319669496466645, -32.00000000000000000, 101.7116913729795300 ) ) ;
#12769 = CARTESIAN_POINT ( 'NONE',  ( -83.20384757729335945, -33.00134618820329990, -96.99999999999997158 ) ) ;
#12770 =( BOUNDED_CURVE ( )  B_SPLINE_CURVE ( 2, ( #17059, #15598, #18918, #17258, #753, #10023, #3765 ),
 .UNSPECIFIED., .F., .F. ) 
 B_SPLINE_CURVE_WITH_KNOTS ( ( 3, 2, 2, 3 ),
 ( 0.8958333333333333703, 0.9027777777777777901, 0.9166666666666666297, 0.9258785066912882389 ),
 .UNSPECIFIED. ) 
 CURVE ( )  GEOMETRIC_REPRESENTATION_ITEM ( )  RATIONAL_B_SPLINE_CURVE ( ( 0.9330127018922192983, 0.9330127018922198534, 1.000000000000000000, 0.8660254037844387076, 1.000000000000000000, 0.9111410165655264848, 0.9401539157124900736 ) ) 
 REPRESENTATION_ITEM ( '' )  );
#12771 = CARTESIAN_POINT ( 'NONE',  ( 233.0909187468005825, -32.00000000000000000, 97.16185054498762952 ) ) ;
#12772 = CARTESIAN_POINT ( 'NONE',  ( 82.40000000000000568, -30.00000000000000355, -96.99999999999998579 ) ) ;
#12773 = CARTESIAN_POINT ( 'NONE',  ( 85.15643035624999868, -30.66562499938548569, -101.5914258081833879 ) ) ;
#12774 = CARTESIAN_POINT ( 'NONE',  ( -82.39999999999999147, -32.98124999877096286, 102.9999999999999858 ) ) ;
#12775 = ORIENTED_EDGE ( 'NONE', *, *, #12327, .T. ) ;
#12776 = CARTESIAN_POINT ( 'NONE',  ( 79.39999999999999147, -30.58124999877096784, 101.7320508075688821 ) ) ;
#12777 = PRODUCT_CONTEXT ( 'NONE', #5707, 'mechanical' ) ;
#12778 = CARTESIAN_POINT ( 'NONE',  ( 235.1663847376154592, -35.00000000000000000, -48.97827398863936565 ) ) ;
#12779 = CARTESIAN_POINT ( 'NONE',  ( 232.5999999999999375, -33.06562499938547717, -53.18285161636690361 ) ) ;
#12780 = CARTESIAN_POINT ( 'NONE',  ( -83.77821517812500929, -32.46562499938548285, 97.61286128772489690 ) ) ;
#12781 = CARTESIAN_POINT ( 'NONE',  ( 229.5999999999999375, -32.69999999999999574, -50.00000000000011369 ) ) ;
#12782 = ORIENTED_EDGE ( 'NONE', *, *, #15458, .T. ) ;
#12783 = CARTESIAN_POINT ( 'NONE',  ( -81.02178482187500208, -30.44062499938548783, -97.61286128772489690 ) ) ;
#12784 = DIRECTION ( 'NONE',  ( -0.000000000000000000, -1.000000000000000000, -0.000000000000000000 ) ) ;
#12785 = ORIENTED_EDGE ( 'NONE', *, *, #13656, .F. ) ;
#12786 = CARTESIAN_POINT ( 'NONE',  ( 79.64356964374999848, -34.52812499938548285, 99.99999999999998579 ) ) ;
#12787 = CARTESIAN_POINT ( 'NONE',  ( -82.39999999999999147, -31.71562499938548640, -103.1828516163667899 ) ) ;
#12788 = CARTESIAN_POINT ( 'NONE',  ( 83.90000000000000568, -34.42500000000000426, 97.40192378864668399 ) ) ;
#12789 = FACE_OUTER_BOUND ( 'NONE', #14166, .T. ) ;
#12790 = CARTESIAN_POINT ( 'NONE',  ( -83.90000000000000568, -31.81874999877096855, 97.40192378864668399 ) ) ;
#12791 = CARTESIAN_POINT ( 'NONE',  ( -82.39999999999999147, -31.71562499938548640, 96.81714838363319586 ) ) ;
#12792 = CARTESIAN_POINT ( 'NONE',  ( -85.15643035625001289, -33.77812499938548285, -101.5914258081833879 ) ) ;
#12793 = PRODUCT ( 'connecting block', 'connecting block', '', ( #2029 ) ) ;
#12794 = DIRECTION ( 'NONE',  ( -0.000000000000000000, -1.000000000000000000, -0.000000000000000000 ) ) ;
#12795 = CARTESIAN_POINT ( 'NONE',  ( 230.7036604445367232, -32.00000000000000711, 102.0295751981966390 ) ) ;
#12796 = CARTESIAN_POINT ( 'NONE',  ( 235.5999999999999943, -30.18749999999999289, 98.26794919243110371 ) ) ;
#12797 = ORIENTED_EDGE ( 'NONE', *, *, #945, .T. ) ;
#12798 = CARTESIAN_POINT ( 'NONE',  ( 85.15643035625001289, -32.87812499938548427, -98.40857419181659793 ) ) ;
#12799 =( NAMED_UNIT ( * ) SI_UNIT ( $, .STERADIAN. ) SOLID_ANGLE_UNIT ( ) );
#12800 = CARTESIAN_POINT ( 'NONE',  ( 235.5999999999999943, -30.65624999877095647, 101.7320508075688537 ) ) ;
#12801 = CARTESIAN_POINT ( 'NONE',  ( 229.5999999999999375, -32.15624999877096002, -48.26794919243123161 ) ) ;
#12802 = EDGE_LOOP ( 'NONE', ( #11886, #14003, #8072, #1931 ) ) ;
#12803 = CARTESIAN_POINT ( 'NONE',  ( -85.40000000000000568, -35.34374999877096712, 99.99999999999998579 ) ) ;
#12804 = CARTESIAN_POINT ( 'NONE',  ( -82.39999999999999147, -30.25312499938548783, 96.81714838363319586 ) ) ;
#12805 = DIRECTION ( 'NONE',  ( -1.000000000000000000, -0.000000000000000000, -0.000000000000000000 ) ) ;
#12806 = ORIENTED_EDGE ( 'NONE', *, *, #12588, .T. ) ;
#12807 = CARTESIAN_POINT ( 'NONE',  ( 4.030867648406119663, -2.329326259789124443, 2.965488570641622523 ) ) ;
#12808 = EDGE_CURVE ( 'NONE', #1356, #18009, #12977, .T. ) ;
#12809 = ORIENTED_EDGE ( 'NONE', *, *, #3608, .F. ) ;
#12810 = CARTESIAN_POINT ( 'NONE',  ( -79.58826230849692251, -32.00000000000093792, -101.0460072438472139 ) ) ;
#12811 = CARTESIAN_POINT ( 'NONE',  ( 80.90000000000000568, -33.00000000000000000, -102.5980762113533018 ) ) ;
#12812 = CARTESIAN_POINT ( 'NONE',  ( 82.40000000000000568, -30.00000000000000355, -103.0000000000000000 ) ) ;
#12813 = EDGE_CURVE ( 'NONE', #2968, #5414, #1358, .T. ) ;
#12814 = EDGE_CURVE ( 'NONE', #11431, #1776, #6137, .T. ) ;
#12815 = CARTESIAN_POINT ( 'NONE',  ( -81.02178482187500208, -32.35312499938548569, 102.3871387122750889 ) ) ;
#12816 = CARTESIAN_POINT ( 'NONE',  ( -82.39999999999999147, -34.60856250001229739, 96.53589838486223584 ) ) ;
#12817 = CARTESIAN_POINT ( 'NONE',  ( -85.40000000000000568, -30.39374999877097139, 99.99999999999998579 ) ) ;
#12818 = DIRECTION ( 'NONE',  ( 0.000000000000000000, 0.000000000000000000, 1.000000000000000000 ) ) ;
#12819 = CARTESIAN_POINT ( 'NONE',  ( 83.77821517812500929, -32.01562499938548001, 102.3871387122750889 ) ) ;
#12820 = CARTESIAN_POINT ( 'NONE',  ( 82.40000000000000568, -33.71249999999998437, 102.9999999999999858 ) ) ;
#12821 = CARTESIAN_POINT ( 'NONE',  ( -79.64356964375001269, -34.82812499938548711, 98.40857419181659793 ) ) ;
#12822 = CARTESIAN_POINT ( 'NONE',  ( -80.90000000000000568, -31.20000000000000284, 102.5980762113533018 ) ) ;
#12823 = ORIENTED_EDGE ( 'NONE', *, *, #8155, .F. ) ;
#12824 = CARTESIAN_POINT ( 'NONE',  ( 81.59615242270662350, -32.83259618943233704, 102.9999999999999716 ) ) ;
#12825 = DIRECTION ( 'NONE',  ( -0.000000000000000000, -0.000000000000000000, 1.000000000000000000 ) ) ;
#12826 = EDGE_CURVE ( 'NONE', #6930, #18607, #13418, .T. ) ;
#12827 = CARTESIAN_POINT ( 'NONE',  ( -3.436319922987618902, 2.634841920961291439, -3.531542292955721862 ) ) ;
#12828 = CARTESIAN_POINT ( 'NONE',  ( 232.5999999999999943, -34.41562499938547859, 96.81714838363319586 ) ) ;
#12829 = CARTESIAN_POINT ( 'NONE',  ( -82.39999999999999147, -33.51562499938548001, 96.81714838363319586 ) ) ;
#12830 = EDGE_CURVE ( 'NONE', #11098, #3049, #4569, .T. ) ;
#12831 = CARTESIAN_POINT ( 'NONE',  ( 229.8435696437499871, -31.52812499938547575, -51.59142580818350865 ) ) ;
#12832 =( BOUNDED_SURFACE ( )  B_SPLINE_SURFACE ( 3, 2, ( 
 ( #12904, #8407, #17403 ),
 ( #11142, #6764, #12709 ),
 ( #12610, #18871, #3812 ),
 ( #6862, #15648, #5493 ),
 ( #15841, #12807, #18680 ),
 ( #6951, #17208, #15932 ) ),
 .UNSPECIFIED., .F., .F., .F. ) 
 B_SPLINE_SURFACE_WITH_KNOTS ( ( 4, 2, 4 ),
 ( 3, 3 ),
 ( 0.01651999345535505592, 0.01858032176739835700, 0.02064065007944165808 ),
 ( 0.000000000000000000, 1.000000000000000000 ),
 .UNSPECIFIED. ) 
 GEOMETRIC_REPRESENTATION_ITEM ( )  RATIONAL_B_SPLINE_SURFACE ( (
 ( 1.000000000000000000, 0.8047781103519390244, 1.000000000000000000),
 ( 1.000000000000000000, 0.8123785825601840260, 1.000000000000000000),
 ( 1.000000000000000000, 0.8190671539791607447, 1.000000000000000000),
 ( 1.000000000000000000, 0.8192352254831567482, 1.000000000000000000),
 ( 1.000000000000000000, 0.8126129677214078972, 1.000000000000000000),
 ( 1.000000000000000000, 0.8047712537969722302, 1.000000000000000000) ) ) 
 REPRESENTATION_ITEM ( '' )  SURFACE ( )  );
#12833 = ORIENTED_EDGE ( 'NONE', *, *, #7219, .T. ) ;
#12834 = CARTESIAN_POINT ( 'NONE',  ( 0.2174200650117532607, 2.185595227304857335, -3.214438021527932676 ) ) ;
#12835 = CARTESIAN_POINT ( 'NONE',  ( -83.77821517812500929, -33.21562499938548285, 102.3871387122750889 ) ) ;
#12836 = CARTESIAN_POINT ( 'NONE',  ( 232.5999999999999375, -29.99999999999999645, -53.00000000000012079 ) ) ;
#12837 = CARTESIAN_POINT ( 'NONE',  ( 82.39999999999999147, -32.05312499938548854, 103.1828516163667899 ) ) ;
#12838 = DIRECTION ( 'NONE',  ( 0.000000000000000000, 0.000000000000000000, -1.000000000000000000 ) ) ;
#12839 = LINE ( 'NONE', #4143, #16719 ) ;
#12840 = CARTESIAN_POINT ( 'NONE',  ( -81.02178482187500208, -34.60312499938549280, 102.3871387122750889 ) ) ;
#12841 = CARTESIAN_POINT ( 'NONE',  ( -83.77821517812500929, -34.37812499938548427, -102.3871387122750889 ) ) ;
#12842 = CARTESIAN_POINT ( 'NONE',  ( 83.77821517812500929, -32.91562499938547859, 102.3871387122750889 ) ) ;
#12843 = CARTESIAN_POINT ( 'NONE',  ( 85.15643035624999868, -34.34062499938548285, -98.40857419181659793 ) ) ;
#12844 = CARTESIAN_POINT ( 'NONE',  ( 233.9782151781249411, -32.54062499938547859, -52.38713871227520968 ) ) ;
#12845 = CARTESIAN_POINT ( 'NONE',  ( -83.77821517812500929, -33.66562499938548569, 102.3871387122750889 ) ) ;
#12846 = CARTESIAN_POINT ( 'NONE',  ( 81.02178482187500208, -30.89062499938548711, -102.3871387122750889 ) ) ;
#12847 = VERTEX_POINT ( 'NONE', #1551 ) ;
#12848 = DIRECTION ( 'NONE',  ( -1.000000000000000000, 0.000000000000000000, 0.000000000000000000 ) ) ;
#12849 = CARTESIAN_POINT ( 'NONE',  ( -0.02448733951239248641, -4.877042772274742255, -3.751161874094027571 ) ) ;
#12850 = CARTESIAN_POINT ( 'NONE',  ( -85.40000000000000568, -34.50000000000000000, 99.99999999999998579 ) ) ;
#12851 = CARTESIAN_POINT ( 'NONE',  ( -79.64356964375001269, -31.75312499938548427, 101.5914258081833879 ) ) ;
#12852 = CARTESIAN_POINT ( 'NONE',  ( -85.15643035624999868, -30.55312499938548854, 101.5914258081833879 ) ) ;
#12853 = CARTESIAN_POINT ( 'NONE',  ( 105.1999999999999886, -29.80000000000001492, -97.80000000000002558 ) ) ;
#12854 = CARTESIAN_POINT ( 'NONE',  ( -83.90000000000000568, -33.67500000000000426, -102.5980762113533018 ) ) ;
#12855 = AXIS2_PLACEMENT_3D ( 'NONE', #4256, #13233, #8741 ) ;
#12856 = CIRCLE ( 'NONE', #19107, 3.000000000000002665 ) ;
#12857 = CARTESIAN_POINT ( 'NONE',  ( -82.40000000000000568, -30.00000000000000355, 103.0000000000000000 ) ) ;
#12858 = CARTESIAN_POINT ( 'NONE',  ( 83.41996205656103314, -34.99999999999999289, -97.17173842519744653 ) ) ;
#12859 = CARTESIAN_POINT ( 'NONE',  ( -83.90000000000000568, -30.97106250001229100, 97.40192378864668399 ) ) ;
#12860 = CARTESIAN_POINT ( 'NONE',  ( 105.1999999999999744, -29.80000000000000071, -100.0000000000000000 ) ) ;
#12861 = EDGE_CURVE ( 'NONE', #2004, #9023, #15021, .T. ) ;
#12862 = CARTESIAN_POINT ( 'NONE',  ( -4.211140560182196957, 2.431303136016537803, -3.745885042887433514 ) ) ;
#12863 = CARTESIAN_POINT ( 'NONE',  ( -83.77821517812500929, -30.66562499938548569, 97.61286128772489690 ) ) ;
#12864 = CARTESIAN_POINT ( 'NONE',  ( -85.40000000000000568, -33.60000000000000142, 99.99999999999998579 ) ) ;
#12865 = CARTESIAN_POINT ( 'NONE',  ( 81.02178482187500208, -30.40312499938548640, 102.3871387122750889 ) ) ;
#12866 = CARTESIAN_POINT ( 'NONE',  ( 232.3828836072648869, -32.00000000000001421, 97.16008101253267171 ) ) ;
#12867 = CARTESIAN_POINT ( 'NONE',  ( 85.15643035624999868, -34.79062499938548569, -98.40857419181659793 ) ) ;
#12868 = DIRECTION ( 'NONE',  ( -1.000000000000000000, 1.586032892321652482E-15, 0.000000000000000000 ) ) ;
#12869 = ORIENTED_EDGE ( 'NONE', *, *, #7677, .F. ) ;
#12870 = CARTESIAN_POINT ( 'NONE',  ( 80.90000000000000568, -33.69374999877096855, 102.5980762113533018 ) ) ;
#12871 = CARTESIAN_POINT ( 'NONE',  ( 233.9782151781249411, -33.70312499938548001, 102.3871387122750889 ) ) ;
#12872 = CARTESIAN_POINT ( 'NONE',  ( 233.9782151781249411, -33.55312499938548143, -52.38713871227520968 ) ) ;
#12873 = CARTESIAN_POINT ( 'NONE',  ( -79.64356964374999848, -30.47812499938548569, 99.99999999999998579 ) ) ;
#12874 = CARTESIAN_POINT ( 'NONE',  ( -85.29357727954830182, -35.00000000000000711, -99.68450386720851952 ) ) ;
#12875 = ORIENTED_EDGE ( 'NONE', *, *, #8279, .T. ) ;
#12876 = CARTESIAN_POINT ( 'NONE',  ( -85.15643035624999868, -31.45312499938548356, -98.40857419181659793 ) ) ;
#12877 = CARTESIAN_POINT ( 'NONE',  ( 83.90000000000000568, -33.07500000000000284, 97.40192378864668399 ) ) ;
#12878 = ORIENTED_EDGE ( 'NONE', *, *, #9240, .F. ) ;
#12879 = CARTESIAN_POINT ( 'NONE',  ( 83.77821517812500929, -32.57812499938548711, 102.3871387122750889 ) ) ;
#12880 = EDGE_CURVE ( 'NONE', #5078, #14237, #9560, .T. ) ;
#12881 = CARTESIAN_POINT ( 'NONE',  ( -79.64356964374999848, -31.37812499938548427, -99.99999999999998579 ) ) ;
#12882 = AXIS2_PLACEMENT_3D ( 'NONE', #10839, #9472, #15243 ) ;
#12883 =( BOUNDED_CURVE ( )  B_SPLINE_CURVE ( 2, ( #7374, #13430, #60, #16177, #8930, #10311, #11865, #13044, #3070 ),
 .UNSPECIFIED., .F., .F. ) 
 B_SPLINE_CURVE_WITH_KNOTS ( ( 3, 2, 2, 2, 3 ),
 ( 0.5208333333333333703, 0.5277777777777777901, 0.5416666666666666297, 0.5555555555555555802, 0.5625000000000000000 ),
 .UNSPECIFIED. ) 
 CURVE ( )  GEOMETRIC_REPRESENTATION_ITEM ( )  RATIONAL_B_SPLINE_CURVE ( ( 0.9330127018922192983, 0.9330127018922198534, 1.000000000000000000, 0.8660254037844387076, 1.000000000000000000, 0.8660254037844387076, 1.000000000000000000, 0.9330127018922194093, 0.9330127018922194093 ) ) 
 REPRESENTATION_ITEM ( '' )  );
#12884 = CARTESIAN_POINT ( 'NONE',  ( -80.90000000000000568, -30.54374999877096997, -102.5980762113533018 ) ) ;
#12885 = CARTESIAN_POINT ( 'NONE',  ( -79.67114894419042059, -35.00000000000001421, 99.22311565912312403 ) ) ;
#12886 = CARTESIAN_POINT ( 'NONE',  ( -80.90000000000000568, -35.19374999877096855, 102.5980762113533018 ) ) ;
#12887 = CARTESIAN_POINT ( 'NONE',  ( -84.69813954184694182, -35.39427337414329600, 98.07164457472185859 ) ) ;
#12888 = CARTESIAN_POINT ( 'NONE',  ( -83.77821517812500929, -32.76562499938548711, -97.61286128772489690 ) ) ;
#12889 = CARTESIAN_POINT ( 'NONE',  ( 235.2218879900010791, -34.99999999999999289, 100.8506536761482124 ) ) ;
#12890 = CARTESIAN_POINT ( 'NONE',  ( 79.39999999999999147, -32.90624999877096712, -101.7320508075688537 ) ) ;
#12891 = CARTESIAN_POINT ( 'NONE',  ( 234.0999999999999375, -31.19999999999999574, 102.5980762113533018 ) ) ;
#12892 = VERTEX_POINT ( 'NONE', #13162 ) ;
#12893 = CARTESIAN_POINT ( 'NONE',  ( 81.02178482187500208, -32.24062499938548854, -102.3871387122750889 ) ) ;
#12894 =( NAMED_UNIT ( * ) PLANE_ANGLE_UNIT ( ) SI_UNIT ( $, .RADIAN. ) );
#12895 = CARTESIAN_POINT ( 'NONE',  ( 229.5999999999999375, -32.64374999877096428, 99.99999999999998579 ) ) ;
#12896 = DIRECTION ( 'NONE',  ( -0.000000000000000000, -1.000000000000000000, -0.000000000000000000 ) ) ;
#12897 = VERTEX_POINT ( 'NONE', #13740 ) ;
#12898 = B_SPLINE_CURVE_WITH_KNOTS ( 'NONE', 3,
 ( #9684, #16916, #17304, #8222, #2450 ),
 .UNSPECIFIED., .F., .F.,
 ( 4, 1, 4 ),
 ( 0.000000000000000000, 0.002020725942163690940, 0.004041451884327382747 ),
 .UNSPECIFIED. ) ;
#12899 = CARTESIAN_POINT ( 'NONE',  ( -85.40000000000000568, -35.36739040097838682, 98.90809659374339446 ) ) ;
#12900 = EDGE_CURVE ( 'NONE', #5530, #14645, #2074, .T. ) ;
#12901 = CARTESIAN_POINT ( 'NONE',  ( -79.64356964374999848, -30.81562499938548427, 99.99999999999998579 ) ) ;
#12902 = CARTESIAN_POINT ( 'NONE',  ( 79.58826230851033756, -31.99999999999998579, 101.0460072438832952 ) ) ;
#12903 = VERTEX_POINT ( 'NONE', #3747 ) ;
#12904 = CARTESIAN_POINT ( 'NONE',  ( 4.086262629614033415, -4.082406995609994205, -0.07093633357110862292 ) ) ;
#12905 = CARTESIAN_POINT ( 'NONE',  ( -82.40000000000000568, -33.65624999877097423, 97.00000000000000000 ) ) ;
#12906 = VERTEX_POINT ( 'NONE', #11269 ) ;
#12907 = CARTESIAN_POINT ( 'NONE',  ( -94.79999999999999716, -29.80000000000000426, 150.0000000000000000 ) ) ;
#12908 = CARTESIAN_POINT ( 'NONE',  ( 85.40000000000000568, -33.11250000000000426, -101.7320508075688679 ) ) ;
#12909 = DIRECTION ( 'NONE',  ( 0.000000000000000000, 0.5000000000000018874, 0.8660254037844375974 ) ) ;
#12910 = CARTESIAN_POINT ( 'NONE',  ( -85.15643035624999868, -31.11562499938548854, 101.5914258081833879 ) ) ;
#12911 = CARTESIAN_POINT ( 'NONE',  ( -85.40000000000000568, -33.18750000000000000, 98.26794919243111792 ) ) ;
#12912 = CARTESIAN_POINT ( 'NONE',  ( -80.90000000000000568, -34.80000000000000426, -97.40192378864668399 ) ) ;
#12913 = CARTESIAN_POINT ( 'NONE',  ( 234.7581833435468184, -31.99999999999999289, -52.02304716543538632 ) ) ;
#12914 = CARTESIAN_POINT ( 'NONE',  ( 85.15643035625001289, -34.79062499938548569, -98.40857419181659793 ) ) ;
#12915 = CARTESIAN_POINT ( 'NONE',  ( -81.59615242270665192, -33.67634618820330417, 97.00000000000000000 ) ) ;
#12916 = CARTESIAN_POINT ( 'NONE',  ( -85.15643035624999868, -34.67812499938548143, 98.40857419181659793 ) ) ;
#12917 = CARTESIAN_POINT ( 'NONE',  ( -80.90000000000000568, -31.05000000000000071, 97.40192378864668399 ) ) ;
#12918 = ORIENTED_EDGE ( 'NONE', *, *, #8174, .F. ) ;
#12919 = CARTESIAN_POINT ( 'NONE',  ( 232.5999999999999375, -34.83749999999999147, -46.53589838486234953 ) ) ;
#12920 = CARTESIAN_POINT ( 'NONE',  ( -82.40000000000000568, -30.00000000000000355, 99.99999999999998579 ) ) ;
#12921 = CARTESIAN_POINT ( 'NONE',  ( -0.6640947660597427138, 4.471078309994878985, -3.602146406945963442 ) ) ;
#12922 = CARTESIAN_POINT ( 'NONE',  ( 233.9782151781249411, -34.00312499938547717, 97.61286128772489690 ) ) ;
#12923 = CARTESIAN_POINT ( 'NONE',  ( -81.02178482187500208, -32.80312499938548854, 102.3871387122750889 ) ) ;
#12924 = CARTESIAN_POINT ( 'NONE',  ( 235.3564303562499447, -30.40312499938547575, -48.40857419181671162 ) ) ;
#12925 = VERTEX_POINT ( 'NONE', #9713 ) ;
#12926 = CARTESIAN_POINT ( 'NONE',  ( -79.64356964375001269, -33.10312499938549280, 101.5914258081833879 ) ) ;
#12927 = CARTESIAN_POINT ( 'NONE',  ( -83.60689295392862164, -35.00000000000000000, -102.7535308243270293 ) ) ;
#12928 = CARTESIAN_POINT ( 'NONE',  ( 79.64356964374999848, -34.86562499938548143, 99.99999999999998579 ) ) ;
#12929 = DIRECTION ( 'NONE',  ( -0.000000000000000000, 0.000000000000000000, -1.000000000000000000 ) ) ;
#12930 = ADVANCED_FACE ( 'NONE', ( #9809 ), #18344, .F. ) ;
#12931 = DIRECTION ( 'NONE',  ( 1.000000000000000000, -0.000000000000000000, -2.407412430484046130E-31 ) ) ;
#12932 = CARTESIAN_POINT ( 'NONE',  ( -85.15643035625001289, -34.79062499938548569, 98.40857419181659793 ) ) ;
#12933 = CARTESIAN_POINT ( 'NONE',  ( -82.39999999999999147, -34.86562499938548854, -103.1828516163667899 ) ) ;
#12934 = CARTESIAN_POINT ( 'NONE',  ( 82.39999999999999147, -32.95312499938548711, 103.1828516163667899 ) ) ;
#12935 = CARTESIAN_POINT ( 'NONE',  ( 83.77821517812500929, -33.47812499938548569, -97.61286128772489690 ) ) ;
#12936 = CARTESIAN_POINT ( 'NONE',  ( 231.2217848218749339, -33.66562499938547859, -47.61286128772501769 ) ) ;
#12937 = CARTESIAN_POINT ( 'NONE',  ( -81.02178482187500208, -34.04062499938548569, 102.3871387122750889 ) ) ;
#12938 = CARTESIAN_POINT ( 'NONE',  ( 83.77821517812500929, -30.51562499938548711, -102.3871387122750889 ) ) ;
#12939 = ADVANCED_FACE ( 'NONE', ( #1729 ), #3059, .T. ) ;
#12940 = VERTEX_POINT ( 'NONE', #15208 ) ;
#12941 = CARTESIAN_POINT ( 'NONE',  ( 85.15643035625001289, -35.20312499938548711, 99.99999999999998579 ) ) ;
#12942 = CARTESIAN_POINT ( 'NONE',  ( 1.243802165048773611, -3.900692638707475624, -3.223146290109810241 ) ) ;
#12943 = CARTESIAN_POINT ( 'NONE',  ( -80.90000000000000568, -32.55000000000000426, 102.5980762113533018 ) ) ;
#12944 = CARTESIAN_POINT ( 'NONE',  ( -82.39999999999999147, -33.40312499938548285, 96.81714838363319586 ) ) ;
#12945 = CARTESIAN_POINT ( 'NONE',  ( -85.15643035624999868, -31.00312499938548072, 101.5914258081833879 ) ) ;
#12946 = DIRECTION ( 'NONE',  ( 0.000000000000000000, 0.000000000000000000, 1.000000000000000000 ) ) ;
#12947 = AXIS2_PLACEMENT_3D ( 'NONE', #17262, #14216, #5252 ) ;
#12948 = PRODUCT_DEFINITION_SHAPE ( 'NONE', 'NONE',  #19333 ) ;
#12949 = CARTESIAN_POINT ( 'NONE',  ( 232.5999999999999943, -32.95312499938548001, 96.81714838363319586 ) ) ;
#12950 = LINE ( 'NONE', #18922, #17656 ) ;
#12951 = CARTESIAN_POINT ( 'NONE',  ( -82.40000000000000568, -30.00000000000000355, 103.0000000000000000 ) ) ;
#12952 = EDGE_CURVE ( 'NONE', #11625, #6661, #932, .T. ) ;
#12953 = CARTESIAN_POINT ( 'NONE',  ( 4.211140560182196957, 2.431303136016536470, -3.745885042887433514 ) ) ;
#12954 = CARTESIAN_POINT ( 'NONE',  ( -84.70388354820684640, -35.00002705695768412, 98.07851859032987818 ) ) ;
#12955 = CARTESIAN_POINT ( 'NONE',  ( -82.39999999999999147, -33.20624999877097849, -102.9999999999999858 ) ) ;
#12956 = CARTESIAN_POINT ( 'NONE',  ( -83.20384757729337366, -33.50759618943233420, 103.0000000000000000 ) ) ;
#12957 = CARTESIAN_POINT ( 'NONE',  ( 85.15643035625001289, -30.25312499938548783, 99.99999999999998579 ) ) ;
#12958 = EDGE_CURVE ( 'NONE', #3780, #18099, #6331, .T. ) ;
#12959 = CARTESIAN_POINT ( 'NONE',  ( 233.5509609210264728, -32.00000000000000000, 97.25957015487007595 ) ) ;
#12960 = CARTESIAN_POINT ( 'NONE',  ( 231.0999999999999375, -34.96874999877096002, -52.59807621135342970 ) ) ;
#12961 = CARTESIAN_POINT ( 'NONE',  ( 81.02178482187500208, -32.65312499938548996, -97.61286128772489690 ) ) ;
#12962 = CARTESIAN_POINT ( 'NONE',  ( 4.151274195509468967, 2.039912954708818837, 3.533232880573625501 ) ) ;
#12963 = AXIS2_PLACEMENT_3D ( 'NONE', #11369, #6979, #13120 ) ;
#12964 = EDGE_LOOP ( 'NONE', ( #8593, #12366 ) ) ;
#12965 = CARTESIAN_POINT ( 'NONE',  ( 80.90000000000000568, -32.79374999877096997, 102.5980762113533018 ) ) ;
#12966 = DIRECTION ( 'NONE',  ( 0.000000000000000000, 0.000000000000000000, 1.000000000000000000 ) ) ;
#12967 = CARTESIAN_POINT ( 'NONE',  ( 229.8435696437499871, -32.46562499938548285, -48.40857419181671162 ) ) ;
#12968 = CARTESIAN_POINT ( 'NONE',  ( 83.20384757729338787, -34.59240381056766722, 102.9999999999999858 ) ) ;
#12969 = DIRECTION ( 'NONE',  ( -1.000000000000000000, 1.586032892321652482E-15, 0.000000000000000000 ) ) ;
#12970 = ORIENTED_EDGE ( 'NONE', *, *, #7452, .T. ) ;
#12971 = EDGE_CURVE ( 'NONE', #15137, #17445, #3366, .T. ) ;
#12972 = CARTESIAN_POINT ( 'NONE',  ( -79.64356964375001269, -33.10312499938549280, -98.40857419181659793 ) ) ;
#12973 = LINE ( 'NONE', #8385, #9110 ) ;
#12974 = EDGE_LOOP ( 'NONE', ( #17305, #990, #11478, #17812 ) ) ;
#12975 = CARTESIAN_POINT ( 'NONE',  ( 82.39999999999999147, -33.29062499938548569, 96.81714838363319586 ) ) ;
#12976 = CARTESIAN_POINT ( 'NONE',  ( -85.15643035624999868, -31.56562499938548427, -98.40857419181659793 ) ) ;
#12977 = CIRCLE ( 'NONE', #12992, 5.199999999999996625 ) ;
#12978 = CARTESIAN_POINT ( 'NONE',  ( 85.40000000000000568, -34.53750000000000142, 101.7320508075688679 ) ) ;
#12979 = CARTESIAN_POINT ( 'NONE',  ( 232.5999999999999375, -30.36562499938548498, 96.81714838363319586 ) ) ;
#12980 = CARTESIAN_POINT ( 'NONE',  ( -79.39999999999999147, -34.25624999877096855, 101.7320508075688537 ) ) ;
#12981 = CARTESIAN_POINT ( 'NONE',  ( -79.64356964375001269, -30.89062499938548711, 98.40857419181659793 ) ) ;
#12982 = CARTESIAN_POINT ( 'NONE',  ( -82.39999999999999147, -32.50312499938548427, -103.1828516163667899 ) ) ;
#12983 = CARTESIAN_POINT ( 'NONE',  ( 234.1913891058629815, -35.00000000000002132, 102.2789443502791045 ) ) ;
#12984 = ADVANCED_FACE ( 'NONE', ( #378 ), #15415, .F. ) ;
#12985 = CARTESIAN_POINT ( 'NONE',  ( 82.39999999999999147, -32.08124999877097139, -103.4641016151377499 ) ) ;
#12986 = CARTESIAN_POINT ( 'NONE',  ( 235.5999999999999375, -30.22499999999999432, 99.99999999999998579 ) ) ;
#12987 = AXIS2_PLACEMENT_3D ( 'NONE', #5863, #16889, #16979 ) ;
#12988 = ORIENTED_EDGE ( 'NONE', *, *, #17971, .F. ) ;
#12989 = CARTESIAN_POINT ( 'NONE',  ( 82.39999999999999147, -34.75312499938548427, -96.81714838363319586 ) ) ;
#12990 = CARTESIAN_POINT ( 'NONE',  ( 229.5999999999999375, -32.68124999877096570, 98.26794919243111792 ) ) ;
#12991 = CARTESIAN_POINT ( 'NONE',  ( 231.0999999999999375, -30.91874999877096286, -52.59807621135342970 ) ) ;
#12992 = AXIS2_PLACEMENT_3D ( 'NONE', #11803, #14722, #13547 ) ;
#12993 = DIRECTION ( 'NONE',  ( -0.000000000000000000, -0.000000000000000000, 1.000000000000000000 ) ) ;
#12994 = CARTESIAN_POINT ( 'NONE',  ( 110.0000000000000000, 10.19999999999997620, -150.0000000000000000 ) ) ;
#12995 = ORIENTED_EDGE ( 'NONE', *, *, #10081, .T. ) ;
#12996 = ORIENTED_EDGE ( 'NONE', *, *, #17168, .T. ) ;
#12997 = CARTESIAN_POINT ( 'NONE',  ( 244.7999999999999545, -29.80000000000001492, -97.80000000000002558 ) ) ;
#12998 =( BOUNDED_CURVE ( )  B_SPLINE_CURVE ( 2, ( #2101, #7771, #6221, #15288, #6407, #267, #18330, #9422, #5042 ),
 .UNSPECIFIED., .F., .F. ) 
 B_SPLINE_CURVE_WITH_KNOTS ( ( 3, 2, 2, 2, 3 ),
 ( 0.5208333333333332593, 0.5277777777777777901, 0.5416666666666666297, 0.5555555555555555802, 0.5625000000000002220 ),
 .UNSPECIFIED. ) 
 CURVE ( )  GEOMETRIC_REPRESENTATION_ITEM ( )  RATIONAL_B_SPLINE_CURVE ( ( 0.9330127018922192983, 0.9330127018922187432, 1.000000000000000000, 0.8660254037844387076, 1.000000000000000000, 0.8660254037844387076, 1.000000000000000000, 0.9330127018922171889, 0.9330127018922194093 ) ) 
 REPRESENTATION_ITEM ( '' )  );
#12999 = CARTESIAN_POINT ( 'NONE',  ( -83.20384757729338787, -32.10134618820330132, 102.9999999999999858 ) ) ;
#13000 = ORIENTED_EDGE ( 'NONE', *, *, #8987, .F. ) ;
#13001 = CARTESIAN_POINT ( 'NONE',  ( 80.90000000000000568, -32.40000000000000568, -97.40192378864668399 ) ) ;
#13002 = DIRECTION ( 'NONE',  ( 0.000000000000000000, 1.000000000000000000, 0.000000000000000000 ) ) ;
#13003 = CARTESIAN_POINT ( 'NONE',  ( 79.58826230851033756, -31.99999999999998579, 101.0460072438832952 ) ) ;
#13004 = CARTESIAN_POINT ( 'NONE',  ( -79.64356964375001269, -32.69062499938548427, 98.40857419181659793 ) ) ;
#13005 = CARTESIAN_POINT ( 'NONE',  ( -85.40000000000000568, -32.21249999999999858, 101.7320508075688679 ) ) ;
#13006 = CARTESIAN_POINT ( 'NONE',  ( -82.40000000000000568, -30.00000000000000355, 103.0000000000000000 ) ) ;
#13007 = AXIS2_PLACEMENT_3D ( 'NONE', #17555, #5736, #9040 ) ;
#13008 = CARTESIAN_POINT ( 'NONE',  ( 232.3828836072649722, -31.99999999999998579, -52.83991898746749172 ) ) ;
#13009 = CARTESIAN_POINT ( 'NONE',  ( 244.7999999999999545, -29.80000000000001492, -97.80000000000002558 ) ) ;
#13010 = CYLINDRICAL_SURFACE ( 'NONE', #6516, 3.000000000000002665 ) ;
#13011 = CARTESIAN_POINT ( 'NONE',  ( -96.99999999999998579, -29.80000000000000426, 150.0000000000000000 ) ) ;
#13012 = CARTESIAN_POINT ( 'NONE',  ( 111.0000000000000000, 10.19999999999997620, -139.9999999999999716 ) ) ;
#13013 = ORIENTED_EDGE ( 'NONE', *, *, #2950, .T. ) ;
#13014 = VECTOR ( 'NONE', #8261, 1000.000000000000000 ) ;
#13015 = CARTESIAN_POINT ( 'NONE',  ( -81.02178482187500208, -30.74062499938548498, -102.3871387122750889 ) ) ;
#13016 = CARTESIAN_POINT ( 'NONE',  ( 232.5999999999999375, -29.99999999999999645, -47.00000000000010658 ) ) ;
#13017 = CYLINDRICAL_SURFACE ( 'NONE', #13940, 3.000000000000002665 ) ;
#13018 = CARTESIAN_POINT ( 'NONE',  ( 231.2217848218749339, -33.92812499938548143, 97.61286128772489690 ) ) ;
#13019 = CARTESIAN_POINT ( 'NONE',  ( -79.64356964374999848, -32.72812499938548569, 99.99999999999998579 ) ) ;
#13020 = DIRECTION ( 'NONE',  ( 0.000000000000000000, -0.000000000000000000, -1.000000000000000000 ) ) ;
#13021 = CARTESIAN_POINT ( 'NONE',  ( 231.2217848218749339, -31.11562499938547788, -52.38713871227520968 ) ) ;
#13022 = VERTEX_POINT ( 'NONE', #12378 ) ;
#13023 = CARTESIAN_POINT ( 'NONE',  ( -83.77821517812500929, -34.11562499938548854, 102.3871387122750889 ) ) ;
#13024 = CARTESIAN_POINT ( 'NONE',  ( -83.90000000000000568, -30.76874999877097139, 102.5980762113533018 ) ) ;
#13025 = CARTESIAN_POINT ( 'NONE',  ( 85.15643035624999868, -35.11426541925033007, 101.0032526477118751 ) ) ;
#13026 = VECTOR ( 'NONE', #5416, 1000.000000000000000 ) ;
#13027 = CARTESIAN_POINT ( 'NONE',  ( 231.0999999999999375, -33.16874999877095576, -52.59807621135342970 ) ) ;
#13028 = CARTESIAN_POINT ( 'NONE',  ( 235.3564303562499447, -31.30312499938547788, 101.5914258081833879 ) ) ;
#13029 = CARTESIAN_POINT ( 'NONE',  ( -83.77821517812500929, -33.32812499938548711, 102.3871387122750889 ) ) ;
#13030 = AXIS2_PLACEMENT_3D ( 'NONE', #14619, #4178, #10138 ) ;
#13031 = CARTESIAN_POINT ( 'NONE',  ( -85.15643035625001289, -32.91562499938548569, -98.40857419181659793 ) ) ;
#13032 = CARTESIAN_POINT ( 'NONE',  ( 79.64356964374999848, -33.51562499938548711, 99.99999999999998579 ) ) ;
#13033 = CARTESIAN_POINT ( 'NONE',  ( 83.77821517812500929, -35.12812499938548427, -102.3871387122750889 ) ) ;
#13034 = CARTESIAN_POINT ( 'NONE',  ( 229.8435696437499303, -31.94062499938547717, -50.00000000000011369 ) ) ;
#13035 = CARTESIAN_POINT ( 'NONE',  ( -81.02178482187500208, -32.69062499938548427, 102.3871387122750889 ) ) ;
#13036 = CARTESIAN_POINT ( 'NONE',  ( 82.39999999999999147, -30.47812499938548569, -103.1828516163667899 ) ) ;
#13037 = ORIENTED_EDGE ( 'NONE', *, *, #12814, .F. ) ;
#13038 = CYLINDRICAL_SURFACE ( 'NONE', #3814, 3.000000000000002665 ) ;
#13039 = CARTESIAN_POINT ( 'NONE',  ( 82.40000000000001990, -33.88124999877096855, 97.00000000000000000 ) ) ;
#13040 = CARTESIAN_POINT ( 'NONE',  ( -85.40000000000000568, -33.11250000000000426, 101.7320508075688679 ) ) ;
#13041 = CARTESIAN_POINT ( 'NONE',  ( -79.64356964375001269, -34.37812499938548427, 98.40857419181659793 ) ) ;
#13042 = CARTESIAN_POINT ( 'NONE',  ( -85.15643035624999868, -31.52812499938547930, 98.40857419181659793 ) ) ;
#13043 = ORIENTED_EDGE ( 'NONE', *, *, #12104, .F. ) ;
#13044 = CARTESIAN_POINT ( 'NONE',  ( -81.59615242270662350, -33.01740381056767148, 102.9999999999999858 ) ) ;
#13045 = AXIS2_PLACEMENT_3D ( 'NONE', #13651, #1924, #10628 ) ;
#13046 = EDGE_CURVE ( 'NONE', #8256, #18958, #7939, .T. ) ;
#13047 = VECTOR ( 'NONE', #15656, 1000.000000000000000 ) ;
#13048 = CARTESIAN_POINT ( 'NONE',  ( 229.8435696437499303, -33.29062499938547148, 99.99999999999998579 ) ) ;
#13049 = LINE ( 'NONE', #7376, #8595 ) ;
#13050 = CARTESIAN_POINT ( 'NONE',  ( -79.39999999999999147, -30.22106250001229100, 99.99999999999998579 ) ) ;
#13051 = EDGE_CURVE ( 'NONE', #18958, #10687, #10825, .T. ) ;
#13052 = CARTESIAN_POINT ( 'NONE',  ( -82.40000000000000568, -34.38749999999999574, 102.9999999999999858 ) ) ;
#13053 = CARTESIAN_POINT ( 'NONE',  ( 0.000000000000000000, 0.000000000000000000, 0.000000000000000000 ) ) ;
#13054 = CARTESIAN_POINT ( 'NONE',  ( -81.59615242270662350, -33.22634618820330843, -102.9999999999999858 ) ) ;
#13055 = CARTESIAN_POINT ( 'NONE',  ( -82.40000000000000568, -33.71249999999998437, 96.99999999999998579 ) ) ;
#13056 = CARTESIAN_POINT ( 'NONE',  ( 81.02178482187500208, -32.80312499938548854, 97.61286128772489690 ) ) ;
#13057 = CARTESIAN_POINT ( 'NONE',  ( 232.5999999999999375, -29.99999999999999645, 96.99999999999998579 ) ) ;
#13058 = CARTESIAN_POINT ( 'NONE',  ( 244.7999999999999545, -32.00000000000000000, 150.0000000000000000 ) ) ;
#13059 = CARTESIAN_POINT ( 'NONE',  ( 79.64356964375001269, -33.66562499938549280, -101.5914258081833879 ) ) ;
#13060 = CIRCLE ( 'NONE', #15563, 2.649999999999982148 ) ;
#13061 = CARTESIAN_POINT ( 'NONE',  ( 232.5999999999999375, -34.16249999999999432, 96.99999999999997158 ) ) ;
#13062 = VERTEX_POINT ( 'NONE', #1405 ) ;
#13063 = CARTESIAN_POINT ( 'NONE',  ( 82.39999999999999147, -32.53124999877096712, 96.53589838486223584 ) ) ;
#13064 = CARTESIAN_POINT ( 'NONE',  ( 232.5999999999999375, -33.96562499938547575, 96.81714838363319586 ) ) ;
#13065 = CARTESIAN_POINT ( 'NONE',  ( 83.90000000000000568, -32.56874999877096855, 97.40192378864668399 ) ) ;
#13066 = EDGE_CURVE ( 'NONE', #2658, #1546, #4911, .T. ) ;
#13067 = CARTESIAN_POINT ( 'NONE',  ( 83.20384757729335945, -34.40759618943233988, 96.99999999999998579 ) ) ;
#13068 = CARTESIAN_POINT ( 'NONE',  ( -82.40000000000000568, -30.00000000000000355, 99.99999999999998579 ) ) ;
#13069 = ORIENTED_EDGE ( 'NONE', *, *, #17408, .F. ) ;
#13070 = CARTESIAN_POINT ( 'NONE',  ( -85.15643035624999868, -33.77812499938548285, -101.5914258081833879 ) ) ;
#13071 = ADVANCED_FACE ( 'NONE', ( #17527 ), #6978, .F. ) ;
#13072 = DIRECTION ( 'NONE',  ( -0.000000000000000000, -1.000000000000000000, -0.000000000000000000 ) ) ;
#13073 = VERTEX_POINT ( 'NONE', #17435 ) ;
#13074 = CARTESIAN_POINT ( 'NONE',  ( -82.39999999999999147, -30.36562499938549209, -103.1828516163667899 ) ) ;
#13075 = CARTESIAN_POINT ( 'NONE',  ( -83.90000000000000568, -31.66874999877096997, -97.40192378864668399 ) ) ;
#13076 = CARTESIAN_POINT ( 'NONE',  ( -85.40000000000000568, -34.40624999877096712, 101.7320508075688679 ) ) ;
#13077 = CARTESIAN_POINT ( 'NONE',  ( -85.15643035624999868, -32.01562499938548711, 101.5914258081833879 ) ) ;
#13078 = CARTESIAN_POINT ( 'NONE',  ( -85.15643035625001289, -32.80312499938548854, -98.40857419181659793 ) ) ;
#13079 = CARTESIAN_POINT ( 'NONE',  ( 229.5999999999999375, -32.24999999999999289, -50.00000000000011369 ) ) ;
#13080 = CARTESIAN_POINT ( 'NONE',  ( 80.90000000000000568, -32.04374999877096997, -102.5980762113533018 ) ) ;
#13081 = CARTESIAN_POINT ( 'NONE',  ( 235.5999999999999375, -32.02499999999999858, 99.99999999999998579 ) ) ;
#13082 = ORIENTED_EDGE ( 'NONE', *, *, #2560, .T. ) ;
#13083 = CARTESIAN_POINT ( 'NONE',  ( 96.99999999999998579, 4.758098676964956264E-15, 150.0000000000000000 ) ) ;
#13084 = SURFACE_STYLE_FILL_AREA ( #19149 ) ;
#13085 = CARTESIAN_POINT ( 'NONE',  ( 229.5999999999999375, -31.70624999877096073, 101.7320508075688679 ) ) ;
#13086 = CARTESIAN_POINT ( 'NONE',  ( 231.0999999999999375, -30.76874999877096428, -47.40192378864679768 ) ) ;
#13087 = CARTESIAN_POINT ( 'NONE',  ( 5.599999999999999645, 2.020725942163686728, -3.499999999999999556 ) ) ;
#13088 = CARTESIAN_POINT ( 'NONE',  ( -81.02178482187500208, -30.89062499938548711, 102.3871387122750889 ) ) ;
#13089 = VERTEX_POINT ( 'NONE', #5619 ) ;
#13090 = VERTEX_POINT ( 'NONE', #18997 ) ;
#13091 = CARTESIAN_POINT ( 'NONE',  ( 79.39999999999999147, -34.23750000000000426, -98.26794919243110371 ) ) ;
#13092 = CARTESIAN_POINT ( 'NONE',  ( 244.7999999999999545, -32.00000000000001421, -103.0000000000000142 ) ) ;
#13093 = VERTEX_POINT ( 'NONE', #11564 ) ;
#13094 = CARTESIAN_POINT ( 'NONE',  ( 82.40000000000001990, -32.53124999877097423, -103.0000000000000000 ) ) ;
#13095 = CARTESIAN_POINT ( 'NONE',  ( 80.90000000000000568, -33.30000000000000426, -97.40192378864668399 ) ) ;
#13096 = EDGE_CURVE ( 'NONE', #5485, #5078, #15960, .T. ) ;
#13097 = PLANE ( 'NONE',  #16428 ) ;
#13098 = CARTESIAN_POINT ( 'NONE',  ( -81.02178482187500208, -31.30312499938548498, 97.61286128772489690 ) ) ;
#13099 = CARTESIAN_POINT ( 'NONE',  ( -83.90000000000000568, -32.32500000000000284, 97.40192378864668399 ) ) ;
#13100 = LINE ( 'NONE', #16237, #11488 ) ;
#13101 = ADVANCED_FACE ( 'NONE', ( #17622 ), #7357, .F. ) ;
#13102 = CARTESIAN_POINT ( 'NONE',  ( -84.69814161231455785, -35.39427329483935836, 98.07164704222793716 ) ) ;
#13103 = CARTESIAN_POINT ( 'NONE',  ( -81.02178482187500208, -34.94062499938548427, 102.3871387122750889 ) ) ;
#13104 = CARTESIAN_POINT ( 'NONE',  ( 244.7999999999999545, -29.80000000000000426, -100.0000000000000000 ) ) ;
#13105 = ORIENTED_EDGE ( 'NONE', *, *, #945, .F. ) ;
#13106 = FILL_AREA_STYLE_COLOUR ( '', #15204 ) ;
#13107 = CARTESIAN_POINT ( 'NONE',  ( -85.15643035625001289, -31.94062499938548427, -99.99999999999998579 ) ) ;
#13108 = CARTESIAN_POINT ( 'NONE',  ( 85.40000000000000568, -34.89374999877097139, 99.99999999999998579 ) ) ;
#13109 = CARTESIAN_POINT ( 'NONE',  ( 232.5999999999999943, -34.19062499938547717, 103.1828516163667899 ) ) ;
#13110 = CARTESIAN_POINT ( 'NONE',  ( -85.15643035625001289, -30.14062499938548711, 99.99999999999998579 ) ) ;
#13111 = FACE_OUTER_BOUND ( 'NONE', #14170, .T. ) ;
#13112 = CARTESIAN_POINT ( 'NONE',  ( 233.9782151781249411, -32.99062499938548143, -52.38713871227520968 ) ) ;
#13113 = VERTEX_POINT ( 'NONE', #4139 ) ;
#13114 = ORIENTED_EDGE ( 'NONE', *, *, #18924, .T. ) ;
#13115 = CARTESIAN_POINT ( 'NONE',  ( -82.39999999999999147, -34.07812499938548711, 103.1828516163667899 ) ) ;
#13116 = DIRECTION ( 'NONE',  ( -0.000000000000000000, -1.000000000000000000, -0.000000000000000000 ) ) ;
#13117 = CARTESIAN_POINT ( 'NONE',  ( 85.15643035624999868, -33.70312499938548711, 98.40857419181659793 ) ) ;
#13118 = DIRECTION ( 'NONE',  ( 0.000000000000000000, 0.000000000000000000, -1.000000000000000000 ) ) ;
#13119 = CARTESIAN_POINT ( 'NONE',  ( 231.2217848218749339, -31.56562499938547717, 97.61286128772489690 ) ) ;
#13120 = DIRECTION ( 'NONE',  ( 0.000000000000000000, 0.000000000000000000, -1.000000000000000000 ) ) ;
#13121 = CARTESIAN_POINT ( 'NONE',  ( -79.39999999999999147, -33.78750000000000853, 98.26794919243110371 ) ) ;
#13122 = CARTESIAN_POINT ( 'NONE',  ( -81.02178482187500208, -33.55312499938548854, -102.3871387122750889 ) ) ;
#13123 = CARTESIAN_POINT ( 'NONE',  ( 79.64356964374999848, -34.86562499938548143, 99.99999999999998579 ) ) ;
#13124 = CARTESIAN_POINT ( 'NONE',  ( 82.39999999999999147, -30.47812499938548569, -103.1828516163667899 ) ) ;
#13125 = CARTESIAN_POINT ( 'NONE',  ( 229.5999999999999375, -31.34999999999999432, -50.00000000000011369 ) ) ;
#13126 = CARTESIAN_POINT ( 'NONE',  ( -79.64356964374998427, -33.02812499938548285, 98.40857419181659793 ) ) ;
#13127 = CARTESIAN_POINT ( 'NONE',  ( 81.02178482187500208, -30.29062499938548569, -97.61286128772489690 ) ) ;
#13128 = VERTEX_POINT ( 'NONE', #8529 ) ;
#13129 = CYLINDRICAL_SURFACE ( 'NONE', #727, 3.000000000000009770 ) ;
#13130 = CARTESIAN_POINT ( 'NONE',  ( 229.8435696437499871, -31.64062499938547290, -51.59142580818350865 ) ) ;
#13131 = CARTESIAN_POINT ( 'NONE',  ( -85.15643035624999868, -33.77812499938548285, 98.40857419181659793 ) ) ;
#13132 = ORIENTED_EDGE ( 'NONE', *, *, #8502, .F. ) ;
#13133 = CARTESIAN_POINT ( 'NONE',  ( 0.000000000000000000, 0.000000000000000000, 0.000000000000000000 ) ) ;
#13134 = CARTESIAN_POINT ( 'NONE',  ( 231.2217848218749339, -33.36562499938548143, 97.61286128772489690 ) ) ;
#13135 = DIRECTION ( 'NONE',  ( 0.9396926207859138680, 1.150791560227856926E-16, -0.3420201433256536139 ) ) ;
#13136 = CARTESIAN_POINT ( 'NONE',  ( 85.40000000000000568, -33.56250000000000000, -101.7320508075688821 ) ) ;
#13137 = CARTESIAN_POINT ( 'NONE',  ( -85.40000000000000568, -34.50000000000000000, 99.99999999999998579 ) ) ;
#13138 = CARTESIAN_POINT ( 'NONE',  ( 234.1936318287815197, -32.00000000000000711, -47.53037344451306012 ) ) ;
#13139 = CARTESIAN_POINT ( 'NONE',  ( -79.64356964374999848, -32.61562499938548854, 99.99999999999998579 ) ) ;
#13140 = CARTESIAN_POINT ( 'NONE',  ( -94.79999999999999716, 0.000000000000000000, 150.0000000000000000 ) ) ;
#13141 = CARTESIAN_POINT ( 'NONE',  ( 82.39999999999999147, -33.74062499938548854, 96.81714838363319586 ) ) ;
#13142 = DIRECTION ( 'NONE',  ( -0.000000000000000000, -1.000000000000000000, -0.000000000000000000 ) ) ;
#13143 = CARTESIAN_POINT ( 'NONE',  ( 105.2000000000000739, -29.80000000000002203, 150.0000000000000000 ) ) ;
#13144 = CARTESIAN_POINT ( 'NONE',  ( 82.39999999999999147, -33.74062499938548854, -103.1828516163667899 ) ) ;
#13145 = CARTESIAN_POINT ( 'NONE',  ( -85.15643035625001289, -31.15312499938548996, -99.99999999999998579 ) ) ;
#13146 = ORIENTED_EDGE ( 'NONE', *, *, #5667, .T. ) ;
#13147 = CARTESIAN_POINT ( 'NONE',  ( 85.40000000000000568, -32.68124999877097281, 101.7320508075688679 ) ) ;
#13148 = CARTESIAN_POINT ( 'NONE',  ( 233.9782151781249411, -34.15312499938547575, 102.3871387122750889 ) ) ;
#13149 = PLANE ( 'NONE',  #14893 ) ;
#13150 = EDGE_CURVE ( 'NONE', #11929, #7231, #9910, .T. ) ;
#13151 = CIRCLE ( 'NONE', #16919, 2.199999999999993516 ) ;
#13152 = EDGE_CURVE ( 'NONE', #7760, #12057, #7350, .T. ) ;
#13153 = CLOSED_SHELL ( 'NONE', ( #15436, #1868, #5200, #6379, #18251, #7845, #2083, #18309, #2062, #1135, #15453, #18667, #2439, #14964, #3066, #12230, #8335, #16441, #15592, #1448, #6426, #14518, #4210, #13767, #16034, #1975, #10710, #1990, #11433, #6973, #2337, #3252, #4828, #6012, #14929, #12208, #13661, #8059, #14850, #12267, #12350, #15081, #13101, #18489, #8552, #10885, #4604, #8522, #13071, #17249, #4965, #4361, #10776, #9099, #5678, #9755, #3160, #18071, #7821, #3844, #17629, #14361, #5962, #9965, #15684, #18920, #5792, #11617, #2590, #1080, #17860, #9122, #2699, #2069, #16793, #8447, #19140, #17802, #15702, #16540, #18807, #13171, #12561, #3742, #14739, #1527, #17715, #1677, #2193, #17225, #10685, #13995, #3156, #17137, #6988, #9950, #9041, #16217, #10694, #14138, #6260, #15587, #1287, #831, #10681, #18072, #1744, #17112 ) ) ;
#13154 = CARTESIAN_POINT ( 'NONE',  ( 234.0999999999999375, -34.14374999877096428, 97.40192378864668399 ) ) ;
#13155 = LINE ( 'NONE', #4274, #1503 ) ;
#13156 = EDGE_LOOP ( 'NONE', ( #12785, #6100, #17980, #12286 ) ) ;
#13157 = CARTESIAN_POINT ( 'NONE',  ( -83.77821517812500929, -34.71562499938548285, -102.3871387122750889 ) ) ;
#13158 = FACE_OUTER_BOUND ( 'NONE', #15934, .T. ) ;
#13159 = ORIENTED_EDGE ( 'NONE', *, *, #8801, .T. ) ;
#13160 = DIRECTION ( 'NONE',  ( 1.000000000000000000, -1.387778780781445676E-15, -2.407412430484046130E-31 ) ) ;
#13161 = CARTESIAN_POINT ( 'NONE',  ( -85.15643035625001289, -30.25312499938548783, -99.99999999999998579 ) ) ;
#13162 = CARTESIAN_POINT ( 'NONE',  ( 235.4117376914898045, -31.99999999999999289, 98.95399275611721635 ) ) ;
#13163 = CARTESIAN_POINT ( 'NONE',  ( -82.39999999999999147, -31.40624999877097068, -103.4641016151377499 ) ) ;
#13164 = CARTESIAN_POINT ( 'NONE',  ( 229.8435696437499871, -32.46562499938548285, 101.5914258081833879 ) ) ;
#13165 = CARTESIAN_POINT ( 'NONE',  ( -85.40000000000000568, -34.48124999877096997, 98.26794919243111792 ) ) ;
#13166 = EDGE_CURVE ( 'NONE', #17250, #7672, #19089, .T. ) ;
#13167 = CARTESIAN_POINT ( 'NONE',  ( -79.64356964375001269, -30.44062499938548783, 98.40857419181659793 ) ) ;
#13168 = CARTESIAN_POINT ( 'NONE',  ( -82.39999999999999147, -33.62812499938548427, -96.81714838363319586 ) ) ;
#13169 = CARTESIAN_POINT ( 'NONE',  ( 82.39999999999999147, -32.58750000000000568, -102.9999999999999858 ) ) ;
#13170 = CIRCLE ( 'NONE', #18792, 5.200000000000001066 ) ;
#13171 = ADVANCED_FACE ( 'NONE', ( #19289 ), #7260, .T. ) ;
#13172 = CARTESIAN_POINT ( 'NONE',  ( 231.0429922824658320, -35.00000000000000711, 97.42750194505826755 ) ) ;
#13173 = CARTESIAN_POINT ( 'NONE',  ( 83.90000000000000568, -31.21874999877097068, -102.5980762113533018 ) ) ;
#13174 = CARTESIAN_POINT ( 'NONE',  ( 234.0999999999999375, -31.04999999999999361, 97.40192378864668399 ) ) ;
#13175 = ORIENTED_EDGE ( 'NONE', *, *, #10900, .T. ) ;
#13176 = CARTESIAN_POINT ( 'NONE',  ( 85.15643035625001289, -34.19062499938548427, -99.99999999999998579 ) ) ;
#13177 = CARTESIAN_POINT ( 'NONE',  ( 235.5999999999999943, -32.90624999877096002, 101.7320508075688537 ) ) ;
#13178 = CARTESIAN_POINT ( 'NONE',  ( 235.5999999999999943, -34.18124999877096570, -51.73205080756900287 ) ) ;
#13179 = EDGE_CURVE ( 'NONE', #16539, #11084, #7236, .T. ) ;
#13180 = CARTESIAN_POINT ( 'NONE',  ( -82.39999999999999147, -32.27812499938548285, 103.1828516163667899 ) ) ;
#13181 = ORIENTED_EDGE ( 'NONE', *, *, #1759, .T. ) ;
#13182 = ORIENTED_EDGE ( 'NONE', *, *, #4818, .F. ) ;
#13183 = CARTESIAN_POINT ( 'NONE',  ( 82.40000000000001990, -34.16250000000000853, -97.00000000000000000 ) ) ;
#13184 = MECHANICAL_DESIGN_GEOMETRIC_PRESENTATION_REPRESENTATION (  '', ( #5710 ), #10990 ) ;
#13185 = CARTESIAN_POINT ( 'NONE',  ( -82.49978216248248941, -35.00000000000000000, -97.23961338448006586 ) ) ;
#13186 = COLOUR_RGB ( '',1.000000000000000000, 0.9490196078431372140, 0.9098039215686274384 ) ;
#13187 = FACE_OUTER_BOUND ( 'NONE', #10045, .T. ) ;
#13188 = ORIENTED_EDGE ( 'NONE', *, *, #12880, .T. ) ;
#13189 = CARTESIAN_POINT ( 'NONE',  ( 79.39999999999999147, -32.45624999877097139, -101.7320508075688537 ) ) ;
#13190 = CARTESIAN_POINT ( 'NONE',  ( 3.972709601346594344, -3.429395227388318812, -1.191688283765307332 ) ) ;
#13191 = DIRECTION ( 'NONE',  ( 1.000000000000000000, -1.387778780781445676E-15, -2.407412430484046130E-31 ) ) ;
#13192 = CARTESIAN_POINT ( 'NONE',  ( -85.15643035624999868, -31.19062499938548783, 98.40857419181659793 ) ) ;
#13193 = CARTESIAN_POINT ( 'NONE',  ( -85.40000000000000568, -32.25000000000000000, 99.99999999999998579 ) ) ;
#13194 = CARTESIAN_POINT ( 'NONE',  ( -82.40000000000000568, -30.00000000000000355, 103.0000000000000000 ) ) ;
#13195 = CARTESIAN_POINT ( 'NONE',  ( 82.40000000000000568, -33.71249999999998437, -96.99999999999998579 ) ) ;
#13196 = LINE ( 'NONE', #4121, #9003 ) ;
#13197 = CARTESIAN_POINT ( 'NONE',  ( -79.64356964375001269, -34.45312499938548711, 101.5914258081833879 ) ) ;
#13198 = AXIS2_PLACEMENT_3D ( 'NONE', #2253, #17013, #2166 ) ;
#13199 = CARTESIAN_POINT ( 'NONE',  ( -82.39999999999999147, -34.33124999877097139, -97.00000000000000000 ) ) ;
#13200 = ORIENTED_EDGE ( 'NONE', *, *, #8651, .F. ) ;
#13201 = CARTESIAN_POINT ( 'NONE',  ( -79.64356964375001269, -31.67812499938548143, -101.5914258081833879 ) ) ;
#13202 = CARTESIAN_POINT ( 'NONE',  ( 2.836893136758676270, 3.208949435745843903, -3.505054077164911241 ) ) ;
#13203 = CARTESIAN_POINT ( 'NONE',  ( 105.1999999999999886, -4.999999999999984013, -100.0000000000000995 ) ) ;
#13204 = CARTESIAN_POINT ( 'NONE',  ( 231.2217848218749339, -33.77812499938547575, 102.3871387122750889 ) ) ;
#13205 = CARTESIAN_POINT ( 'NONE',  ( -81.02178482187500208, -30.74062499938548498, 97.61286128772489690 ) ) ;
#13206 = CARTESIAN_POINT ( 'NONE',  ( -82.40000000000000568, -50.00000000000000000, 99.99999999999998579 ) ) ;
#13207 = CARTESIAN_POINT ( 'NONE',  ( 232.5999999999999375, -33.85312499938547859, -53.18285161636690361 ) ) ;
#13208 = ORIENTED_EDGE ( 'NONE', *, *, #7571, .T. ) ;
#13209 = VERTEX_POINT ( 'NONE', #16255 ) ;
#13210 = FACE_OUTER_BOUND ( 'NONE', #12605, .T. ) ;
#13211 = EDGE_CURVE ( 'NONE', #9169, #7775, #11754, .T. ) ;
#13212 = CARTESIAN_POINT ( 'NONE',  ( -79.39999999999999147, -30.22500000000000142, 99.99999999999998579 ) ) ;
#13213 = CARTESIAN_POINT ( 'NONE',  ( 113.0000000000000000, 10.39615242270649453, -145.0000000000000000 ) ) ;
#13214 = CARTESIAN_POINT ( 'NONE',  ( 85.40000000000000568, -30.00000000000000355, 99.99999999999998579 ) ) ;
#13215 = CARTESIAN_POINT ( 'NONE',  ( 83.90000000000000568, -34.12500000000000000, -97.40192378864668399 ) ) ;
#13216 = CARTESIAN_POINT ( 'NONE',  ( 235.3564303562499447, -30.77812499938547575, 98.40857419181659793 ) ) ;
#13217 = CARTESIAN_POINT ( 'NONE',  ( 229.8435696437499587, -33.25312499938547717, -48.40857419181671162 ) ) ;
#13218 = CARTESIAN_POINT ( 'NONE',  ( -82.39999999999999147, -30.78750000000000142, 102.9999999999999858 ) ) ;
#13219 = CARTESIAN_POINT ( 'NONE',  ( 83.77821517812500929, -34.26562499938548711, 102.3871387122750889 ) ) ;
#13220 =( BOUNDED_CURVE ( )  B_SPLINE_CURVE ( 2, ( #15214, #4777, #1830, #6620, #16970, #12287, #12569, #3683, #13835 ),
 .UNSPECIFIED., .F., .F. ) 
 B_SPLINE_CURVE_WITH_KNOTS ( ( 3, 2, 2, 2, 3 ),
 ( 0.4791666666666665186, 0.4861111111111111049, 0.5000000000000000000, 0.5138888888888888395, 0.5208333333333333703 ),
 .UNSPECIFIED. ) 
 CURVE ( )  GEOMETRIC_REPRESENTATION_ITEM ( )  RATIONAL_B_SPLINE_CURVE ( ( 0.9330127018922194093, 0.9330127018922180770, 1.000000000000000000, 0.8660254037844387076, 1.000000000000000000, 0.8660254037844387076, 1.000000000000000000, 0.9330127018922187432, 0.9330127018922192983 ) ) 
 REPRESENTATION_ITEM ( '' )  );
#13221 = CARTESIAN_POINT ( 'NONE',  ( 83.77821517812500929, -30.51562499938548711, -102.3871387122750889 ) ) ;
#13222 = CARTESIAN_POINT ( 'NONE',  ( 229.5999999999999375, -30.93749999999999289, -51.73205080756898866 ) ) ;
#13223 = CARTESIAN_POINT ( 'NONE',  ( -80.90000000000000568, -31.44374999877096855, 97.40192378864668399 ) ) ;
#13224 = EDGE_LOOP ( 'NONE', ( #1279, #13000, #7875, #1635 ) ) ;
#13225 = EDGE_CURVE ( 'NONE', #19255, #16126, #3944, .T. ) ;
#13226 = CARTESIAN_POINT ( 'NONE',  ( 82.39999999999999147, -35.09062499938548285, 96.81714838363319586 ) ) ;
#13227 = CYLINDRICAL_SURFACE ( 'NONE', #2114, 7.500000000000020428 ) ;
#13228 = CARTESIAN_POINT ( 'NONE',  ( 232.5999999999999375, -30.59062499938547930, -46.81714838363331666 ) ) ;
#13229 = CARTESIAN_POINT ( 'NONE',  ( -79.64356964375001269, -32.65312499938548285, 101.5914258081833879 ) ) ;
#13230 = ORIENTED_EDGE ( 'NONE', *, *, #13179, .T. ) ;
#13231 = CARTESIAN_POINT ( 'NONE',  ( -84.06832524826180020, -35.00000000000001421, 102.2567273996599226 ) ) ;
#13232 = UNCERTAINTY_MEASURE_WITH_UNIT (LENGTH_MEASURE( 1.000000000000000082E-05 ), #17901, 'distance_accuracy_value', 'NONE');
#13233 = DIRECTION ( 'NONE',  ( -0.000000000000000000, -1.000000000000000000, -0.000000000000000000 ) ) ;
#13234 = DIRECTION ( 'NONE',  ( 0.000000000000000000, -0.000000000000000000, 1.000000000000000000 ) ) ;
#13235 = CARTESIAN_POINT ( 'NONE',  ( -82.39999999999999147, -31.68356250001229313, 103.4641016151377499 ) ) ;
#13236 = CARTESIAN_POINT ( 'NONE',  ( -85.40000000000000568, -33.14999999999999858, -99.99999999999998579 ) ) ;
#13237 = CARTESIAN_POINT ( 'NONE',  ( 232.1383900424028752, -31.99999999999999289, -47.18959324165065539 ) ) ;
#13238 = CARTESIAN_POINT ( 'NONE',  ( -82.39999999999999147, -32.72812499938548569, 103.1828516163667899 ) ) ;
#13239 = CARTESIAN_POINT ( 'NONE',  ( -85.40000000000000568, -32.60624999877096997, 101.7320508075688821 ) ) ;
#13240 = CARTESIAN_POINT ( 'NONE',  ( 82.39999999999999147, -32.84062499938548996, 96.81714838363319586 ) ) ;
#13241 = CARTESIAN_POINT ( 'NONE',  ( 79.68596062386926349, -32.00000000000000000, 98.72172371342817598 ) ) ;
#13242 = ADVANCED_FACE ( 'NONE', ( #16547 ), #9200, .T. ) ;
#13243 = CARTESIAN_POINT ( 'NONE',  ( 229.5999999999999375, -33.14999999999999147, -50.00000000000011369 ) ) ;
#13244 = CARTESIAN_POINT ( 'NONE',  ( 85.15643035624999868, -34.26562499938548711, -101.5914258081833879 ) ) ;
#13245 = CARTESIAN_POINT ( 'NONE',  ( -83.77821517812500929, -30.77812499938548640, -102.3871387122750889 ) ) ;
#13246 = ORIENTED_EDGE ( 'NONE', *, *, #5667, .F. ) ;
#13247 = CARTESIAN_POINT ( 'NONE',  ( 85.40000000000000568, -33.09374999877096712, 99.99999999999998579 ) ) ;
#13248 = CONTEXT_DEPENDENT_SHAPE_REPRESENTATION ( #12198, #9504 ) ;
#13249 = CARTESIAN_POINT ( 'NONE',  ( 2.059999999999998721, 0.000000000000000000, -0.3080913168122742518 ) ) ;
#13250 = CARTESIAN_POINT ( 'NONE',  ( 232.5999999999999375, -34.83749999999999147, -47.00000000000011369 ) ) ;
#13251 = CARTESIAN_POINT ( 'NONE',  ( 83.90000000000000568, -34.57500000000000284, 102.5980762113533018 ) ) ;
#13252 = CARTESIAN_POINT ( 'NONE',  ( 81.59615242270665192, -33.67634618820330417, -97.00000000000000000 ) ) ;
#13253 = ORIENTED_EDGE ( 'NONE', *, *, #4469, .F. ) ;
#13254 = CARTESIAN_POINT ( 'NONE',  ( -81.02178482187500208, -32.99062499938548854, -102.3871387122750889 ) ) ;
#13255 = CARTESIAN_POINT ( 'NONE',  ( -82.40000000000001990, -32.75624999877096855, 97.00000000000000000 ) ) ;
#13256 = ORIENTED_EDGE ( 'NONE', *, *, #6194, .T. ) ;
#13257 = CARTESIAN_POINT ( 'NONE',  ( -81.59615242270660929, -30.31740381056766509, 102.9999999999999858 ) ) ;
#13258 = CARTESIAN_POINT ( 'NONE',  ( -79.64356964375001269, -33.14062499938548711, -101.5914258081833879 ) ) ;
#13259 = CARTESIAN_POINT ( 'NONE',  ( -83.52022063337570046, -32.00000000000000000, -102.5731757466075180 ) ) ;
#13260 = CARTESIAN_POINT ( 'NONE',  ( -85.40000000000000568, -31.25624999877096855, -98.26794919243111792 ) ) ;
#13261 = CARTESIAN_POINT ( 'NONE',  ( 229.8435696437499303, -32.05312499938548143, 99.99999999999998579 ) ) ;
#13262 = CARTESIAN_POINT ( 'NONE',  ( -82.39999999999999147, -34.10624999877096997, 96.53589838486223584 ) ) ;
#13263 = CARTESIAN_POINT ( 'NONE',  ( -79.64356964375001269, -34.56562499938549138, 101.5914258081833879 ) ) ;
#13264 = CARTESIAN_POINT ( 'NONE',  ( -85.40000000000000568, -33.58124999877097139, 98.26794919243111792 ) ) ;
#13265 = CARTESIAN_POINT ( 'NONE',  ( -82.40000000000000568, -30.00000000000000355, 96.99999999999998579 ) ) ;
#13266 =( BOUNDED_CURVE ( )  B_SPLINE_CURVE ( 2, ( #19178, #11745, #17712, #2856, #8813, #19277, #15348, #9383, #12033 ),
 .UNSPECIFIED., .F., .F. ) 
 B_SPLINE_CURVE_WITH_KNOTS ( ( 3, 2, 2, 2, 3 ),
 ( 0.6041666666666666297, 0.6111111111111111605, 0.6250000000000000000, 0.6388888888888888395, 0.6458333333333332593 ),
 .UNSPECIFIED. ) 
 CURVE ( )  GEOMETRIC_REPRESENTATION_ITEM ( )  RATIONAL_B_SPLINE_CURVE ( ( 0.9330127018922192983, 0.9330127018922187432, 1.000000000000000000, 0.8660254037844387076, 1.000000000000000000, 0.8660254037844387076, 1.000000000000000000, 0.9330127018922198534, 0.9330127018922192983 ) ) 
 REPRESENTATION_ITEM ( '' )  );
#13267 = CYLINDRICAL_SURFACE ( 'NONE', #547, 3.000000000000002665 ) ;
#13268 = CARTESIAN_POINT ( 'NONE',  ( 85.40000000000000568, -30.80624999877096926, -101.7320508075688679 ) ) ;
#13269 = CARTESIAN_POINT ( 'NONE',  ( 232.5999999999999375, -32.81249999999999289, 96.53589838486223584 ) ) ;
#13270 = VERTEX_POINT ( 'NONE', #13702 ) ;
#13271 = CARTESIAN_POINT ( 'NONE',  ( 82.05869624310412291, -34.96883842999723413, -102.9857998004475235 ) ) ;
#13272 = CARTESIAN_POINT ( 'NONE',  ( 235.5999999999999943, -34.70624999877096428, 101.7320508075688537 ) ) ;
#13273 = CARTESIAN_POINT ( 'NONE',  ( 235.5999999999999943, -33.80624999877096570, -48.26794919243124582 ) ) ;
#13274 = CARTESIAN_POINT ( 'NONE',  ( -83.77821517812500929, -32.76562499938548711, 102.3871387122750889 ) ) ;
#13275 = VERTEX_POINT ( 'NONE', #6195 ) ;
#13276 = VERTEX_POINT ( 'NONE', #6094 ) ;
#13277 = DIRECTION ( 'NONE',  ( -1.000000000000000000, 1.586032892321652482E-15, -0.000000000000000000 ) ) ;
#13278 = CIRCLE ( 'NONE', #16399, 3.500000000000000000 ) ;
#13279 = CARTESIAN_POINT ( 'NONE',  ( -4.000000000000000000, -0.8382240730041925492, -3.220610619767135141 ) ) ;
#13280 = CARTESIAN_POINT ( 'NONE',  ( 4.197393957002303999, 7.772902908466098641E-14, -3.503767560748929810 ) ) ;
#13281 = ORIENTED_EDGE ( 'NONE', *, *, #8045, .F. ) ;
#13282 = CARTESIAN_POINT ( 'NONE',  ( -83.20384757729335945, -31.83615380933863648, 96.99999999999997158 ) ) ;
#13283 = DIRECTION ( 'NONE',  ( 0.000000000000000000, -1.000000000000000000, 0.000000000000000000 ) ) ;
#13284 = DIRECTION ( 'NONE',  ( 1.000000000000000000, 0.000000000000000000, 4.625929269271481378E-15 ) ) ;
#13285 = CARTESIAN_POINT ( 'NONE',  ( -85.15643035624999868, -33.89062499938548711, 98.40857419181659793 ) ) ;
#13286 = CARTESIAN_POINT ( 'NONE',  ( -85.40000000000000568, -33.14999999999999858, 99.99999999999998579 ) ) ;
#13287 = CARTESIAN_POINT ( 'NONE',  ( -82.39999999999999147, -32.08124999877097139, 103.4641016151377499 ) ) ;
#13288 = DIRECTION ( 'NONE',  ( -0.000000000000000000, -1.000000000000000000, -0.000000000000000000 ) ) ;
#13289 = EDGE_CURVE ( 'NONE', #19014, #4990, #14438, .T. ) ;
#13290 = CARTESIAN_POINT ( 'NONE',  ( 110.0000000000000000, 10.19999999999997620, -139.9999999999999716 ) ) ;
#13291 = CARTESIAN_POINT ( 'NONE',  ( -82.17437583783130606, -35.00000000000002132, -102.9802575795477537 ) ) ;
#13292 = VECTOR ( 'NONE', #4916, 1000.000000000000000 ) ;
#13293 = FACE_OUTER_BOUND ( 'NONE', #19305, .T. ) ;
#13294 = EDGE_LOOP ( 'NONE', ( #13627, #17703, #11235, #14538 ) ) ;
#13295 = CARTESIAN_POINT ( 'NONE',  ( -79.64356964374999848, -34.97812499938548569, -99.99999999999998579 ) ) ;
#13296 = CARTESIAN_POINT ( 'NONE',  ( 235.5999999999999943, -32.51249999999999574, -48.26794919243124582 ) ) ;
#13297 =( BOUNDED_CURVE ( )  B_SPLINE_CURVE ( 3, ( #14388, #1113, #9810, #836 ),
 .UNSPECIFIED., .F., .F. ) 
 B_SPLINE_CURVE_WITH_KNOTS ( ( 4, 4 ),
 ( 4.136407476936552641, 4.745086877030337824 ),
 .UNSPECIFIED. ) 
 CURVE ( )  GEOMETRIC_REPRESENTATION_ITEM ( )  RATIONAL_B_SPLINE_CURVE ( ( 1.000000000000000000, 0.9693633521240625495, 0.9693633521240625495, 1.000000000000000000 ) ) 
 REPRESENTATION_ITEM ( '' )  );
#13298 = LINE ( 'NONE', #5788, #240 ) ;
#13300 = CARTESIAN_POINT ( 'NONE',  ( 244.7999999999999545, -32.00000000000000000, 150.0000000000000000 ) ) ;
#13299 = B_SPLINE_CURVE_WITH_KNOTS ( 'NONE', 3,
 ( #12418, #802, #18387, #10947 ),
 .UNSPECIFIED., .F., .F.,
 ( 4, 4 ),
 ( 2.380739282773697217E-07, 0.002044882221487522803 ),
 .UNSPECIFIED. ) ;
#13301 = CARTESIAN_POINT ( 'NONE',  ( -79.64356964375001269, -31.22812499938548925, 98.40857419181659793 ) ) ;
#13302 = CARTESIAN_POINT ( 'NONE',  ( -84.65149424414151724, -35.03567958137573868, 98.11078664818333550 ) ) ;
#13303 = EDGE_CURVE ( 'NONE', #4877, #5441, #15163, .T. ) ;
#13304 = CARTESIAN_POINT ( 'NONE',  ( 235.3564303562499447, -33.96562499938547575, -50.00000000000011369 ) ) ;
#13305 = CARTESIAN_POINT ( 'NONE',  ( -85.15643035624999868, -32.09062499938548996, 98.40857419181659793 ) ) ;
#13307 = ADVANCED_FACE ( 'NONE', ( #10765 ), #2959, .T. ) ;
#13306 = ORIENTED_EDGE ( 'NONE', *, *, #18097, .T. ) ;
#13308 = ORIENTED_EDGE ( 'NONE', *, *, #4701, .F. ) ;
#13309 = PLANE ( 'NONE',  #437 ) ;
#13310 = CARTESIAN_POINT ( 'NONE',  ( -79.39999999999999147, -31.98750000000000071, 98.26794919243110371 ) ) ;
#13311 = EDGE_CURVE ( 'NONE', #11864, #18009, #14977, .T. ) ;
#13312 = CARTESIAN_POINT ( 'NONE',  ( -79.39999999999999147, -31.06874999877096855, 99.99999999999998579 ) ) ;
#13313 = CARTESIAN_POINT ( 'NONE',  ( 81.02178482187500208, -34.49062499938548854, 97.61286128772489690 ) ) ;
#13314 = CARTESIAN_POINT ( 'NONE',  ( -82.39999999999999147, -32.58750000000000568, 102.9999999999999858 ) ) ;
#13315 = CARTESIAN_POINT ( 'NONE',  ( 229.8435696437499871, -31.90312499938547575, 101.5914258081833879 ) ) ;
#13316 = VECTOR ( 'NONE', #444, 999.9999999999998863 ) ;
#13317 = CARTESIAN_POINT ( 'NONE',  ( 85.15643035625001289, -34.64062499938548711, 99.99999999999998579 ) ) ;
#13318 = CARTESIAN_POINT ( 'NONE',  ( 81.02178482187500208, -30.74062499938548498, -97.61286128772489690 ) ) ;
#13319 = EDGE_CURVE ( 'NONE', #18970, #12892, #15223, .T. ) ;
#13320 = CARTESIAN_POINT ( 'NONE',  ( 233.9782151781249411, -34.79062499938547859, -52.38713871227520968 ) ) ;
#13321 = CARTESIAN_POINT ( 'NONE',  ( -85.15643035625001289, -34.67812499938548143, 98.40857419181659793 ) ) ;
#13322 = CARTESIAN_POINT ( 'NONE',  ( 85.15643035625001289, -33.74062499938548854, -99.99999999999998579 ) ) ;
#13323 = VECTOR ( 'NONE', #10435, 1000.000000000000000 ) ;
#13324 = ORIENTED_EDGE ( 'NONE', *, *, #5431, .F. ) ;
#13325 = DIRECTION ( 'NONE',  ( -0.000000000000000000, -0.000000000000000000, -1.000000000000000000 ) ) ;
#13326 = CARTESIAN_POINT ( 'NONE',  ( 80.90000000000000568, -33.75000000000000000, -97.40192378864668399 ) ) ;
#13327 = CARTESIAN_POINT ( 'NONE',  ( -84.69814068649969840, -35.00052333152936512, 98.07164593887567605 ) ) ;
#13328 = CARTESIAN_POINT ( 'NONE',  ( -85.40000000000000568, -30.45000000000000284, 99.99999999999998579 ) ) ;
#13329 = EDGE_LOOP ( 'NONE', ( #8805, #6255, #14522, #9881 ) ) ;
#13330 = CARTESIAN_POINT ( 'NONE',  ( -4.000000000000000000, 2.309401076758498483, -5.000000000000000000 ) ) ;
#13331 = CONICAL_SURFACE ( 'NONE', #1471, 3.500000000000000000, 1.047197551196600296 ) ;
#13332 = CARTESIAN_POINT ( 'NONE',  ( -81.59615242270665192, -34.18259618943233136, 97.00000000000000000 ) ) ;
#13333 = FACE_OUTER_BOUND ( 'NONE', #6876, .T. ) ;
#13334 = CARTESIAN_POINT ( 'NONE',  ( -79.39999999999999147, -32.92106250001229739, 99.99999999999998579 ) ) ;
#13335 = EDGE_CURVE ( 'NONE', #10447, #12229, #5903, .T. ) ;
#13336 = VECTOR ( 'NONE', #17946, 1000.000000000000000 ) ;
#13337 =( BOUNDED_CURVE ( )  B_SPLINE_CURVE ( 2, ( #8894, #8997, #13486, #18186, #1674, #127, #4808, #19266, #12125 ),
 .UNSPECIFIED., .F., .F. ) 
 B_SPLINE_CURVE_WITH_KNOTS ( ( 3, 2, 2, 2, 3 ),
 ( 0.7708333333333331483, 0.7777777777777777901, 0.7916666666666666297, 0.8055555555555555802, 0.8125000000000001110 ),
 .UNSPECIFIED. ) 
 CURVE ( )  GEOMETRIC_REPRESENTATION_ITEM ( )  RATIONAL_B_SPLINE_CURVE ( ( 0.9330127018922194093, 0.9330127018922177440, 1.000000000000000000, 0.8660254037844387076, 1.000000000000000000, 0.8660254037844387076, 1.000000000000000000, 0.9330127018922182991, 0.9330127018922194093 ) ) 
 REPRESENTATION_ITEM ( '' )  );
#13338 = FACE_OUTER_BOUND ( 'NONE', #9754, .T. ) ;
#13339 = CARTESIAN_POINT ( 'NONE',  ( -79.39999999999999147, -32.38124999877096855, 98.26794919243110371 ) ) ;
#13340 = CARTESIAN_POINT ( 'NONE',  ( -85.15643035624999868, -32.35312499938549280, 101.5914258081833879 ) ) ;
#13341 = CARTESIAN_POINT ( 'NONE',  ( 233.4038475772933623, -32.11740381056766580, 103.0000000000000000 ) ) ;
#13342 = CARTESIAN_POINT ( 'NONE',  ( 85.15643035625001289, -32.05312499938548854, 99.99999999999998579 ) ) ;
#13343 = CARTESIAN_POINT ( 'NONE',  ( 82.40000000000000568, -30.00000000000000355, 103.0000000000000000 ) ) ;
#13344 = CIRCLE ( 'NONE', #5867, 5.560781378645573980 ) ;
#13345 = EDGE_CURVE ( 'NONE', #7737, #17378, #10712, .T. ) ;
#13346 = DIRECTION ( 'NONE',  ( 1.000000000000000000, -0.000000000000000000, -2.407412430484046130E-31 ) ) ;
#13347 = CARTESIAN_POINT ( 'NONE',  ( -85.15643035624999868, -32.02817623523065294, 101.0587761908873290 ) ) ;
#13348 = CARTESIAN_POINT ( 'NONE',  ( -79.64356964375001269, -31.41562499938548569, -98.40857419181659793 ) ) ;
#13349 = VERTEX_POINT ( 'NONE', #17916 ) ;
#13350 = CARTESIAN_POINT ( 'NONE',  ( 84.69813954184694182, -35.39427337414329600, 101.9283554252781272 ) ) ;
#13351 = DIRECTION ( 'NONE',  ( -0.000000000000000000, 1.000000000000000000, -0.000000000000000000 ) ) ;
#13352 = CARTESIAN_POINT ( 'NONE',  ( 229.8435696437499871, -34.34062499938547575, -51.59142580818350865 ) ) ;
#13353 = VECTOR ( 'NONE', #2548, 1000.000000000000000 ) ;
#13354 = VECTOR ( 'NONE', #721, 1000.000000000000000 ) ;
#13355 = CARTESIAN_POINT ( 'NONE',  ( -85.15643035624999868, -32.01562499938548711, 101.5914258081833879 ) ) ;
#13356 = DIRECTION ( 'NONE',  ( -0.000000000000000000, -1.000000000000000000, -0.000000000000000000 ) ) ;
#13357 = ORIENTED_EDGE ( 'NONE', *, *, #18220, .F. ) ;
#13358 = CARTESIAN_POINT ( 'NONE',  ( -83.88339518848731302, -35.16733441503058089, -102.5204086375588162 ) ) ;
#13359 = DIRECTION ( 'NONE',  ( 0.000000000000000000, 0.000000000000000000, -1.000000000000000000 ) ) ;
#13360 = CARTESIAN_POINT ( 'NONE',  ( -85.40000000000000568, -32.15624999877096712, 101.7320508075688821 ) ) ;
#13361 = CIRCLE ( 'NONE', #9934, 10.00000000000000000 ) ;
#13362 = CARTESIAN_POINT ( 'NONE',  ( -81.02178482187500208, -33.25312499938548427, -97.61286128772489690 ) ) ;
#13363 = CARTESIAN_POINT ( 'NONE',  ( -82.85293433256504159, -32.00000000000002132, -102.8010948079636080 ) ) ;
#13364 = CARTESIAN_POINT ( 'NONE',  ( -85.40000000000000568, -30.88124999877097210, -101.7320508075688679 ) ) ;
#13365 = CARTESIAN_POINT ( 'NONE',  ( 231.2217848218749339, -32.57812499938548001, 97.61286128772489690 ) ) ;
#13366 = CARTESIAN_POINT ( 'NONE',  ( -82.39999999999999147, -31.63518749875868252, 103.4641016151377499 ) ) ;
#13367 = CARTESIAN_POINT ( 'NONE',  ( -81.02178482187500208, -33.55312499938548854, 97.61286128772489690 ) ) ;
#13368 = CARTESIAN_POINT ( 'NONE',  ( -81.02178482187500208, -34.94062499938548427, -97.61286128772489690 ) ) ;
#13369 = CARTESIAN_POINT ( 'NONE',  ( 83.77821517812500929, -34.26562499938548711, 102.3871387122750889 ) ) ;
#13370 = PLANE ( 'NONE',  #5559 ) ;
#13371 = CARTESIAN_POINT ( 'NONE',  ( 235.5999999999999375, -33.31874999877096144, 99.99999999999998579 ) ) ;
#13372 = CARTESIAN_POINT ( 'NONE',  ( 83.90000000000000568, -33.91874999877096997, -102.5980762113533018 ) ) ;
#13373 = CARTESIAN_POINT ( 'NONE',  ( 235.5999999999999943, -32.51249999999998863, 101.7320508075688537 ) ) ;
#13374 = VERTEX_POINT ( 'NONE', #3242 ) ;
#13375 = CARTESIAN_POINT ( 'NONE',  ( 79.64356964374998427, -34.90312499938548285, -101.5914258081833879 ) ) ;
#13376 = CARTESIAN_POINT ( 'NONE',  ( 235.3564303562499447, -30.44062499938548072, 98.40857419181659793 ) ) ;
#13377 = CARTESIAN_POINT ( 'NONE',  ( 235.5999999999999375, -33.76874999877096428, -50.00000000000011369 ) ) ;
#13378 = CARTESIAN_POINT ( 'NONE',  ( -85.15643035625001289, -34.19062499938548427, 99.99999999999998579 ) ) ;
#13379 = EDGE_LOOP ( 'NONE', ( #8, #3829, #14290, #5013 ) ) ;
#13380 = ORIENTED_EDGE ( 'NONE', *, *, #11986, .T. ) ;
#13381 = DIRECTION ( 'NONE',  ( -0.000000000000000000, 0.000000000000000000, -1.000000000000000000 ) ) ;
#13382 = CARTESIAN_POINT ( 'NONE',  ( -83.90000000000000568, -34.87500000000000000, 102.5980762113533018 ) ) ;
#13383 = CARTESIAN_POINT ( 'NONE',  ( -85.40000000000000568, -32.15624999877096712, 101.7320508075688821 ) ) ;
#13384 = ORIENTED_EDGE ( 'NONE', *, *, #3904, .T. ) ;
#13385 = CARTESIAN_POINT ( 'NONE',  ( -83.20395887649198130, -35.00000000000002132, 102.6365808225363025 ) ) ;
#13386 = CARTESIAN_POINT ( 'NONE',  ( -3.264624719419710521E-13, -4.796980096169328966, -3.721999068284310486 ) ) ;
#13387 = CARTESIAN_POINT ( 'NONE',  ( -83.77821517812500929, -33.32812499938548711, 102.3871387122750889 ) ) ;
#13388 = CARTESIAN_POINT ( 'NONE',  ( -85.40000000000000568, -30.80624999877096926, 101.7320508075688679 ) ) ;
#13389 =( BOUNDED_CURVE ( )  B_SPLINE_CURVE ( 1, ( #2946, #16533 ),
 .UNSPECIFIED., .F., .F. ) 
 B_SPLINE_CURVE_WITH_KNOTS ( ( 2, 2 ),
 ( 0.000000000000000000, 1.000000000000000000 ),
 .UNSPECIFIED. ) 
 CURVE ( )  GEOMETRIC_REPRESENTATION_ITEM ( )  RATIONAL_B_SPLINE_CURVE ( ( 0.9401539645359766606, 0.9401539645359766606 ) ) 
 REPRESENTATION_ITEM ( '' )  );
#13390 = CARTESIAN_POINT ( 'NONE',  ( -79.39999999999999147, -30.65624999877096712, 101.7320508075688537 ) ) ;
#13391 = CARTESIAN_POINT ( 'NONE',  ( 229.5999999999999375, -33.56249999999999289, 101.7320508075688821 ) ) ;
#13392 = CARTESIAN_POINT ( 'NONE',  ( -82.40000000000000568, -30.00000000000000355, 99.99999999999998579 ) ) ;
#13393 = DIRECTION ( 'NONE',  ( 1.000000000000000000, 0.000000000000000000, 0.000000000000000000 ) ) ;
#13394 =( BOUNDED_SURFACE ( )  B_SPLINE_SURFACE ( 3, 2, ( 
 ( #3644, #11889, #2997 ),
 ( #4471, #10523, #3092 ),
 ( #9053, #16387, #8953 ),
 ( #15018, #1637, #17536 ),
 ( #14489, #6897, #14686 ),
 ( #7177, #14590, #7269 ) ),
 .UNSPECIFIED., .F., .F., .F. ) 
 B_SPLINE_SURFACE_WITH_KNOTS ( ( 4, 2, 4 ),
 ( 3, 3 ),
 ( 0.01652267773200353021, 0.01858309280828997212, 0.02064350788457641403 ),
 ( 0.000000000000000000, 1.000000000000000000 ),
 .UNSPECIFIED. ) 
 GEOMETRIC_REPRESENTATION_ITEM ( )  RATIONAL_B_SPLINE_SURFACE ( (
 ( 1.000000000000000000, 0.8047780975688292315, 1.000000000000000000),
 ( 1.000000000000000000, 0.8123789546324567956, 1.000000000000000000),
 ( 1.000000000000000000, 0.8190677982988761041, 1.000000000000000000),
 ( 1.000000000000000000, 0.8192346069552172150, 1.000000000000000000),
 ( 1.000000000000000000, 0.8126126759768910190, 1.000000000000000000),
 ( 1.000000000000000000, 0.8047712639312011307, 1.000000000000000000) ) ) 
 REPRESENTATION_ITEM ( '' )  SURFACE ( )  );
#13395 = CARTESIAN_POINT ( 'NONE',  ( 232.5999999999999375, -31.15312499938547930, 96.81714838363319586 ) ) ;
#13396 = ORIENTED_EDGE ( 'NONE', *, *, #913, .F. ) ;
#13397 =( NAMED_UNIT ( * ) PLANE_ANGLE_UNIT ( ) SI_UNIT ( $, .RADIAN. ) );
#13398 = CARTESIAN_POINT ( 'NONE',  ( -79.64356964375001269, -33.10312499938549280, -98.40857419181659793 ) ) ;
#13399 = CARTESIAN_POINT ( 'NONE',  ( 233.4038475772932770, -33.41115380933862156, -47.00000000000009948 ) ) ;
#13400 = CARTESIAN_POINT ( 'NONE',  ( -82.40000000000000568, -30.00000000000000355, -103.0000000000000000 ) ) ;
#13401 = CARTESIAN_POINT ( 'NONE',  ( 79.83361526238435601, -35.00000000000000711, -101.0217260113603572 ) ) ;
#13402 = CARTESIAN_POINT ( 'NONE',  ( -81.02178482187500208, -32.24062499938548854, 102.3871387122750889 ) ) ;
#13403 = FACE_OUTER_BOUND ( 'NONE', #3435, .T. ) ;
#13404 = CARTESIAN_POINT ( 'NONE',  ( 231.2217848218749339, -31.86562499938547788, -47.61286128772501769 ) ) ;
#13405 = EDGE_CURVE ( 'NONE', #14097, #11379, #15670, .T. ) ;
#13406 = EDGE_CURVE ( 'NONE', #11406, #4621, #17731, .T. ) ;
#13407 = ORIENTED_EDGE ( 'NONE', *, *, #3268, .F. ) ;
#13408 = VERTEX_POINT ( 'NONE', #3821 ) ;
#13409 = CARTESIAN_POINT ( 'NONE',  ( -85.11512745526620449, -32.00000000000000000, 100.5952676699193802 ) ) ;
#13410 = CARTESIAN_POINT ( 'NONE',  ( -83.90000000000000568, -30.82500000000000284, 102.5980762113533018 ) ) ;
#13411 = CARTESIAN_POINT ( 'NONE',  ( -85.40000000000000568, -31.74374999877096926, 99.99999999999998579 ) ) ;
#13412 = CARTESIAN_POINT ( 'NONE',  ( 85.40000000000000568, -31.76249999999999929, 98.26794919243111792 ) ) ;
#13413 = DIRECTION ( 'NONE',  ( 0.000000000000000000, 0.000000000000000000, 1.000000000000000000 ) ) ;
#13414 = CARTESIAN_POINT ( 'NONE',  ( 232.5999999999999375, -33.40312499938547575, 96.81714838363319586 ) ) ;
#13415 = CARTESIAN_POINT ( 'NONE',  ( 233.9782151781249411, -33.89062499938548001, -52.38713871227520968 ) ) ;
#13416 = CARTESIAN_POINT ( 'NONE',  ( 85.15643035624999868, -35.11426555956768425, 101.0032586025029815 ) ) ;
#13417 = EDGE_CURVE ( 'NONE', #9315, #15126, #16836, .T. ) ;
#13418 =( BOUNDED_CURVE ( )  B_SPLINE_CURVE ( 2, ( #7400, #14925, #17959, #17863, #6044, #5945, #7209, #3096, #12087 ),
 .UNSPECIFIED., .F., .F. ) 
 B_SPLINE_CURVE_WITH_KNOTS ( ( 3, 2, 2, 2, 3 ),
 ( 0.5625000000000001110, 0.5694444444444444198, 0.5833333333333333703, 0.5972222222222222099, 0.6041666666666667407 ),
 .UNSPECIFIED. ) 
 CURVE ( )  GEOMETRIC_REPRESENTATION_ITEM ( )  RATIONAL_B_SPLINE_CURVE ( ( 0.9330127018922194093, 0.9330127018922204085, 1.000000000000000000, 0.8660254037844387076, 1.000000000000000000, 0.8660254037844387076, 1.000000000000000000, 0.9330127018922187432, 0.9330127018922192983 ) ) 
 REPRESENTATION_ITEM ( '' )  );
#13419 = CARTESIAN_POINT ( 'NONE',  ( 85.15643035624999868, -31.52812499938547930, -98.40857419181659793 ) ) ;
#13420 = ORIENTED_EDGE ( 'NONE', *, *, #5795, .T. ) ;
#13421 = CARTESIAN_POINT ( 'NONE',  ( 232.5999999999999375, -34.75312499938547717, -53.18285161636690361 ) ) ;
#13422 = EDGE_CURVE ( 'NONE', #5491, #2466, #7429, .T. ) ;
#13423 = CARTESIAN_POINT ( 'NONE',  ( 105.1999999999999886, -4.999999999999984013, -100.0000000000000995 ) ) ;
#13424 = CARTESIAN_POINT ( 'NONE',  ( 85.15643035624999868, -34.22812499938547859, -98.40857419181659793 ) ) ;
#13425 = DIRECTION ( 'NONE',  ( 0.000000000000000000, 0.000000000000000000, -1.000000000000000000 ) ) ;
#13426 = CARTESIAN_POINT ( 'NONE',  ( 232.5999999999999375, -29.99999999999999645, 99.99999999999998579 ) ) ;
#13427 = CARTESIAN_POINT ( 'NONE',  ( -83.90000000000000568, -34.87500000000000000, 102.5980762113533018 ) ) ;
#13428 = CARTESIAN_POINT ( 'NONE',  ( -79.39999999999999147, -30.22500000000000142, 99.99999999999998579 ) ) ;
#13429 = VERTEX_POINT ( 'NONE', #13885 ) ;
#13430 = CARTESIAN_POINT ( 'NONE',  ( -81.59615242270662350, -32.83259618943233704, 96.99999999999998579 ) ) ;
#13431 = CARTESIAN_POINT ( 'NONE',  ( 231.2217848218749339, -34.71562499938547575, 97.61286128772489690 ) ) ;
#13432 = LINE ( 'NONE', #3166, #15786 ) ;
#13433 = CARTESIAN_POINT ( 'NONE',  ( -83.90000000000000568, -33.07106250001229597, 102.5980762113533018 ) ) ;
#13434 = CARTESIAN_POINT ( 'NONE',  ( 82.40000000000001990, -32.30624999877097281, -97.00000000000000000 ) ) ;
#13435 = CARTESIAN_POINT ( 'NONE',  ( 117.5000000000000142, 12.69999999999998508, 110.0000000000000142 ) ) ;
#13436 = CARTESIAN_POINT ( 'NONE',  ( -82.39999999999999147, -32.27812499938548285, 103.1828516163667899 ) ) ;
#13437 = CARTESIAN_POINT ( 'NONE',  ( -80.90000000000000568, -33.00000000000000000, 102.5980762113533018 ) ) ;
#13438 = CARTESIAN_POINT ( 'NONE',  ( 85.15643035625001289, -31.60312499938548569, 99.99999999999998579 ) ) ;
#13439 = FACE_OUTER_BOUND ( 'NONE', #18522, .T. ) ;
#13440 = CARTESIAN_POINT ( 'NONE',  ( -81.02178482187500208, -32.65312499938548996, 97.61286128772489690 ) ) ;
#13441 = CARTESIAN_POINT ( 'NONE',  ( -85.15643035625001289, -30.70312499938548711, -99.99999999999998579 ) ) ;
#13442 = ORIENTED_EDGE ( 'NONE', *, *, #17045, .F. ) ;
#13443 = CARTESIAN_POINT ( 'NONE',  ( 85.40000000000000568, -34.85624999877096997, 98.26794919243111792 ) ) ;
#13444 = DIRECTION ( 'NONE',  ( -0.000000000000000000, -1.000000000000000000, -0.000000000000000000 ) ) ;
#13445 = CARTESIAN_POINT ( 'NONE',  ( 232.5999999999999375, -34.41562499938547859, -53.18285161636690361 ) ) ;
#13446 = CARTESIAN_POINT ( 'NONE',  ( 4.151274195509469855, -2.039912954708825943, -3.533232880573625057 ) ) ;
#13447 = CARTESIAN_POINT ( 'NONE',  ( -85.15643035625001289, -32.05312499938548854, 99.99999999999998579 ) ) ;
#13448 = CARTESIAN_POINT ( 'NONE',  ( 84.11496519894906498, -31.99999999999998579, 102.1846009218925104 ) ) ;
#13449 = ORIENTED_EDGE ( 'NONE', *, *, #9393, .F. ) ;
#13450 = CARTESIAN_POINT ( 'NONE',  ( -83.90000000000000568, -30.07499999999999929, -102.5980762113533018 ) ) ;
#13451 =( BOUNDED_CURVE ( )  B_SPLINE_CURVE ( 2, ( #3, #11899, #98, #3008, #14633, #17870, #5757, #10533, #13169 ),
 .UNSPECIFIED., .F., .F. ) 
 B_SPLINE_CURVE_WITH_KNOTS ( ( 3, 2, 2, 2, 3 ),
 ( 0.4375000000000000555, 0.4444444444444444198, 0.4583333333333333148, 0.4722222222222222099, 0.4791666666666666297 ),
 .UNSPECIFIED. ) 
 CURVE ( )  GEOMETRIC_REPRESENTATION_ITEM ( )  RATIONAL_B_SPLINE_CURVE ( ( 0.9330127018922192983, 0.9330127018922198534, 1.000000000000000000, 0.8660254037844387076, 1.000000000000000000, 0.8660254037844387076, 1.000000000000000000, 0.9330127018922196314, 0.9330127018922194093 ) ) 
 REPRESENTATION_ITEM ( '' )  );
#13452 = CARTESIAN_POINT ( 'NONE',  ( 4.000000000001088907, 1.658577278524410170, -3.531553309554541720 ) ) ;
#13453 = DIRECTION ( 'NONE',  ( -0.000000000000000000, -1.000000000000000000, -0.000000000000000000 ) ) ;
#13454 = EDGE_CURVE ( 'NONE', #11219, #12136, #8321, .T. ) ;
#13455 = CARTESIAN_POINT ( 'NONE',  ( -79.64356964375001269, -33.21562499938548996, -98.40857419181659793 ) ) ;
#13456 = DIRECTION ( 'NONE',  ( -0.000000000000000000, -1.000000000000000000, -0.000000000000000000 ) ) ;
#13457 = CARTESIAN_POINT ( 'NONE',  ( 232.5999999999999375, -31.49062499938547788, 103.1828516163667899 ) ) ;
#13458 = CARTESIAN_POINT ( 'NONE',  ( -79.39999999999999147, -32.83518749875868536, 98.26794919243110371 ) ) ;
#13459 = CARTESIAN_POINT ( 'NONE',  ( -85.15643035625001289, -32.95312499938548711, 99.99999999999998579 ) ) ;
#13460 = CARTESIAN_POINT ( 'NONE',  ( 232.5999999999999375, -33.65624999877096002, 97.00000000000000000 ) ) ;
#13461 = CARTESIAN_POINT ( 'NONE',  ( 82.39999999999999147, -32.72812499938548569, 96.81714838363319586 ) ) ;
#13462 = FACE_OUTER_BOUND ( 'NONE', #12351, .T. ) ;
#13463 = DIRECTION ( 'NONE',  ( -0.000000000000000000, -0.000000000000000000, -1.000000000000000000 ) ) ;
#13464 = CARTESIAN_POINT ( 'NONE',  ( 79.39999999999999147, -33.31874999877096855, -99.99999999999998579 ) ) ;
#13465 = CARTESIAN_POINT ( 'NONE',  ( 235.5999999999999943, -32.88749999999998863, 98.26794919243110371 ) ) ;
#13466 = EDGE_LOOP ( 'NONE', ( #9557, #6436, #10942, #7087 ) ) ;
#13467 = CARTESIAN_POINT ( 'NONE',  ( 233.9782151781249411, -34.15312499938547575, -47.61286128772501769 ) ) ;
#13468 = CARTESIAN_POINT ( 'NONE',  ( 235.3564303562499447, -30.47812499938547859, 99.99999999999998579 ) ) ;
#13469 = CARTESIAN_POINT ( 'NONE',  ( 234.0999999999999375, -32.94374999877096144, -47.40192378864679768 ) ) ;
#13471 = EDGE_CURVE ( 'NONE', #17889, #927, #12721, .T. ) ;
#13470 = CARTESIAN_POINT ( 'NONE',  ( -85.15643035625001289, -34.64062499938548711, 99.99999999999998579 ) ) ;
#13472 = EDGE_LOOP ( 'NONE', ( #19127, #10738, #17138 ) ) ;
#13473 = VERTEX_POINT ( 'NONE', #2262 ) ;
#13474 = CARTESIAN_POINT ( 'NONE',  ( 4.071447262713890680, -4.041451884327388555, 0.000000000000000000 ) ) ;
#13475 = CARTESIAN_POINT ( 'NONE',  ( -79.39999999999999147, -34.18124999877097281, 98.26794919243110371 ) ) ;
#13476 = CARTESIAN_POINT ( 'NONE',  ( 4.132952817037863547, -4.063368025374529680, 2.739218076410093718E-16 ) ) ;
#13477 = ORIENTED_EDGE ( 'NONE', *, *, #8503, .F. ) ;
#13478 = LINE ( 'NONE', #118, #176 ) ;
#13479 = AXIS2_PLACEMENT_3D ( 'NONE', #18656, #4182, #11602 ) ;
#13480 = CARTESIAN_POINT ( 'NONE',  ( -81.02178482187500208, -33.25312499938548427, 102.3871387122750889 ) ) ;
#13481 = CARTESIAN_POINT ( 'NONE',  ( -79.39999999999999147, -34.23750000000000426, 98.26794919243110371 ) ) ;
#13482 = CARTESIAN_POINT ( 'NONE',  ( -83.90000000000000568, -32.56874999877096855, 102.5980762113533018 ) ) ;
#13483 = CARTESIAN_POINT ( 'NONE',  ( 82.40000000000001990, -32.75624999877096855, 103.0000000000000000 ) ) ;
#13484 = DIRECTION ( 'NONE',  ( 0.000000000000000000, 0.000000000000000000, -1.000000000000000000 ) ) ;
#13485 = CARTESIAN_POINT ( 'NONE',  ( 82.40000000000000568, -30.00000000000000355, 99.99999999999998579 ) ) ;
#13486 = CARTESIAN_POINT ( 'NONE',  ( -80.90000000000000568, -34.59374999877096712, -102.5980762113533018 ) ) ;
#13487 = CARTESIAN_POINT ( 'NONE',  ( -85.40000000000000568, -34.40624999877096712, -98.26794919243111792 ) ) ;
#13488 = EDGE_LOOP ( 'NONE', ( #12462, #18140, #19063, #8525 ) ) ;
#13489 = EDGE_CURVE ( 'NONE', #11146, #4397, #17340, .T. ) ;
#13490 = CARTESIAN_POINT ( 'NONE',  ( -85.15643035624999868, -33.32812499938548001, -101.5914258081833879 ) ) ;
#13491 = CARTESIAN_POINT ( 'NONE',  ( 4.235886605889389145, 2.417314728048528760, -3.751161874094018245 ) ) ;
#13492 = CIRCLE ( 'NONE', #726, 2.055000000000000160 ) ;
#13493 = AXIS2_PLACEMENT_3D ( 'NONE', #14064, #6457, #13967 ) ;
#13494 = CARTESIAN_POINT ( 'NONE',  ( 2.344047193898588954, 3.265465875126468021, -5.031375706690542042E-16 ) ) ;
#13495 = CARTESIAN_POINT ( 'NONE',  ( 82.32247963938024782, -34.99999999999999289, -102.7610832838413444 ) ) ;
#13496 = CARTESIAN_POINT ( 'NONE',  ( -85.15643035624999868, -31.07812499938548356, 98.40857419181659793 ) ) ;
#13497 = CARTESIAN_POINT ( 'NONE',  ( 83.20384757729335945, -33.24240381056766580, -96.99999999999998579 ) ) ;
#13498 = CARTESIAN_POINT ( 'NONE',  ( 235.3564303562499447, -32.12812499938547717, -51.59142580818350865 ) ) ;
#13499 = VERTEX_POINT ( 'NONE', #12333 ) ;
#13500 = ORIENTED_EDGE ( 'NONE', *, *, #8076, .T. ) ;
#13501 = CARTESIAN_POINT ( 'NONE',  ( -82.39999999999999147, -34.83749999999999858, -96.53589838486223584 ) ) ;
#13502 = CARTESIAN_POINT ( 'NONE',  ( -79.39999999999999147, -30.67500000000000071, 99.99999999999998579 ) ) ;
#13503 = CARTESIAN_POINT ( 'NONE',  ( -80.90000000000000568, -32.79374999877096997, 97.40192378864668399 ) ) ;
#13504 = CARTESIAN_POINT ( 'NONE',  ( 80.90000000000000568, -31.20000000000000284, 97.40192378864668399 ) ) ;
#13505 = CARTESIAN_POINT ( 'NONE',  ( -84.29633955546280788, -32.00000000000001421, -97.97042480180299151 ) ) ;
#13507 = CARTESIAN_POINT ( 'NONE',  ( 229.8435696437499871, -34.67812499938547433, 98.40857419181659793 ) ) ;
#13506 = VECTOR ( 'NONE', #19155, 1000.000000000000000 ) ;
#13508 =( BOUNDED_CURVE ( )  B_SPLINE_CURVE ( 2, ( #4972, #10913, #16879, #5062, #3483, #3583, #10127, #11397, #17170 ),
 .UNSPECIFIED., .F., .F. ) 
 B_SPLINE_CURVE_WITH_KNOTS ( ( 3, 2, 2, 2, 3 ),
 ( 0.7291666666666666297, 0.7361111111111111605, 0.7500000000000000000, 0.7638888888888888395, 0.7708333333333331483 ),
 .UNSPECIFIED. ) 
 CURVE ( )  GEOMETRIC_REPRESENTATION_ITEM ( )  RATIONAL_B_SPLINE_CURVE ( ( 0.9330127018922192983, 0.9330127018922187432, 1.000000000000000000, 0.8660254037844387076, 1.000000000000000000, 0.8660254037844387076, 1.000000000000000000, 0.9330127018922209636, 0.9330127018922194093 ) ) 
 REPRESENTATION_ITEM ( '' )  );
#13509 = CARTESIAN_POINT ( 'NONE',  ( 83.20384757729338787, -32.10134618820330132, 97.00000000000000000 ) ) ;
#13510 = CARTESIAN_POINT ( 'NONE',  ( -80.90000000000000568, -32.04374999877096997, -97.40192378864668399 ) ) ;
#13511 = CARTESIAN_POINT ( 'NONE',  ( 79.64356964374999848, -31.26562499938548356, -99.99999999999998579 ) ) ;
#13512 = ORIENTED_EDGE ( 'NONE', *, *, #11727, .F. ) ;
#13513 = CARTESIAN_POINT ( 'NONE',  ( 231.0999999999999375, -30.37499999999999645, -47.40192378864679768 ) ) ;
#13514 = PLANE ( 'NONE',  #18499 ) ;
#13515 = CARTESIAN_POINT ( 'NONE',  ( 82.39999999999999147, -32.50312499938548427, -96.81714838363319586 ) ) ;
#13516 = CARTESIAN_POINT ( 'NONE',  ( 249.9999999999999716, -5.000000000000004441, 150.0000000000000000 ) ) ;
#13517 = FACE_OUTER_BOUND ( 'NONE', #12488, .T. ) ;
#13518 = CARTESIAN_POINT ( 'NONE',  ( -83.33080762004576059, -35.05289549976084373, 96.44210921874548603 ) ) ;
#13519 = CARTESIAN_POINT ( 'NONE',  ( -83.90000000000000568, -30.97500000000000142, 97.40192378864668399 ) ) ;
#13520 = VERTEX_POINT ( 'NONE', #1977 ) ;
#13521 = CARTESIAN_POINT ( 'NONE',  ( -85.16220480609818821, -34.99999999999999289, 98.91314642829009074 ) ) ;
#13522 = CARTESIAN_POINT ( 'NONE',  ( 229.8435696437499587, -34.60312499938547859, 101.5914258081833879 ) ) ;
#13523 = DIRECTION ( 'NONE',  ( -0.000000000000000000, -0.000000000000000000, -1.000000000000000000 ) ) ;
#13524 = CARTESIAN_POINT ( 'NONE',  ( -83.90000000000000568, -32.32106250001229597, 97.40192378864668399 ) ) ;
#13525 = CARTESIAN_POINT ( 'NONE',  ( -79.58826230849687988, -32.00000000000094502, 98.95399275615287138 ) ) ;
#13526 = CARTESIAN_POINT ( 'NONE',  ( -81.59615242270662350, -32.06115380933863435, 103.0000000000000000 ) ) ;
#13527 = CARTESIAN_POINT ( 'NONE',  ( 231.7960411235079050, -35.00000000000002132, 102.6365808225362883 ) ) ;
#13528 = CARTESIAN_POINT ( 'NONE',  ( 79.64356964374999848, -34.97812499938548569, 99.99999999999998579 ) ) ;
#13529 = EDGE_CURVE ( 'NONE', #17007, #800, #9219, .T. ) ;
#13530 = CARTESIAN_POINT ( 'NONE',  ( 105.1999999999999744, -31.99999999999999289, 150.0000000000000000 ) ) ;
#13531 = DIRECTION ( 'NONE',  ( 0.000000000000000000, 0.000000000000000000, -1.000000000000000000 ) ) ;
#13532 = CARTESIAN_POINT ( 'NONE',  ( -82.39999999999999147, -31.49062499938548854, -96.81714838363319586 ) ) ;
#13533 = VERTEX_POINT ( 'NONE', #8231 ) ;
#13534 = CARTESIAN_POINT ( 'NONE',  ( 81.02178482187500208, -31.00312499938548783, 97.61286128772489690 ) ) ;
#13535 = FACE_OUTER_BOUND ( 'NONE', #7605, .T. ) ;
#13536 = DIRECTION ( 'NONE',  ( -0.7071067811865505703, 0.000000000000000000, 0.7071067811865444641 ) ) ;
#13537 = CARTESIAN_POINT ( 'NONE',  ( -81.02178482187500208, -30.55312499938548854, 102.3871387122750889 ) ) ;
#13538 = DIRECTION ( 'NONE',  ( -1.000000000000000000, 0.000000000000000000, 0.000000000000000000 ) ) ;
#13539 = ORIENTED_EDGE ( 'NONE', *, *, #8289, .F. ) ;
#13540 = CARTESIAN_POINT ( 'NONE',  ( -85.40000000000000568, -30.00000000000000355, -99.99999999999998579 ) ) ;
#13541 = B_SPLINE_CURVE_WITH_KNOTS ( 'NONE', 3,
 ( #14365, #1189, #8600, #14551, #4114 ),
 .UNSPECIFIED., .F., .F.,
 ( 4, 1, 4 ),
 ( 0.000000000000000000, 0.002309401076758505790, 0.004618802153517011580 ),
 .UNSPECIFIED. ) ;
#13542 = CARTESIAN_POINT ( 'NONE',  ( 4.000000000000000000, -0.8732470631449981147, -3.223155494240760088 ) ) ;
#13543 = EDGE_CURVE ( 'NONE', #779, #3049, #2099, .T. ) ;
#13544 = CARTESIAN_POINT ( 'NONE',  ( -4.000000000000000000, 2.309401076758498483, -5.000000000000000000 ) ) ;
#13545 = CARTESIAN_POINT ( 'NONE',  ( -79.64356964375001269, -32.24062499938548854, -101.5914258081833879 ) ) ;
#13546 = EDGE_CURVE ( 'NONE', #7994, #9630, #2436, .T. ) ;
#13547 = DIRECTION ( 'NONE',  ( 1.000000000000000000, 0.000000000000000000, 0.000000000000000000 ) ) ;
#13548 = CARTESIAN_POINT ( 'NONE',  ( 233.9782151781249411, -31.75312499938547717, 97.61286128772489690 ) ) ;
#13549 = CARTESIAN_POINT ( 'NONE',  ( -79.39999999999999147, -31.97268749875867400, 99.99999999999998579 ) ) ;
#13550 = CARTESIAN_POINT ( 'NONE',  ( -85.15643035624999868, -33.44062499938548427, 98.40857419181659793 ) ) ;
#13551 = CARTESIAN_POINT ( 'NONE',  ( -79.64356964374998427, -34.45312499938548711, -98.40857419181659793 ) ) ;
#13552 = CARTESIAN_POINT ( 'NONE',  ( 85.15643035625001289, -33.25312499938548427, 98.40857419181659793 ) ) ;
#13553 = CARTESIAN_POINT ( 'NONE',  ( -82.40000000000000568, -30.00000000000000355, 96.99999999999998579 ) ) ;
#13554 = CARTESIAN_POINT ( 'NONE',  ( 83.90000000000000568, -33.16874999877096286, -97.40192378864668399 ) ) ;
#13555 = CARTESIAN_POINT ( 'NONE',  ( 232.5999999999999375, -34.38749999999999574, 103.4641016151377499 ) ) ;
#13556 = ORIENTED_EDGE ( 'NONE', *, *, #14832, .F. ) ;
#13557 = CARTESIAN_POINT ( 'NONE',  ( 235.3564303562499447, -34.49062499938548143, -51.59142580818350154 ) ) ;
#13558 = DIRECTION ( 'NONE',  ( 1.000000000000000000, 0.000000000000000000, 0.000000000000000000 ) ) ;
#13559 = EDGE_CURVE ( 'NONE', #12219, #3413, #10864, .T. ) ;
#13560 = CARTESIAN_POINT ( 'NONE',  ( 229.8435696437499871, -30.29062499938548214, 98.40857419181659793 ) ) ;
#13561 = CARTESIAN_POINT ( 'NONE',  ( 234.0999999999999375, -33.84374999877096002, -47.40192378864679768 ) ) ;
#13562 = CARTESIAN_POINT ( 'NONE',  ( -81.02178482187500208, -32.99062499938548854, 97.61286128772489690 ) ) ;
#13563 = ORIENTED_EDGE ( 'NONE', *, *, #2937, .F. ) ;
#13564 = ORIENTED_EDGE ( 'NONE', *, *, #1328, .T. ) ;
#13565 = CARTESIAN_POINT ( 'NONE',  ( 4.175813232069146785, 2.061359961916366057, -3.570380186727397653 ) ) ;
#13566 = CARTESIAN_POINT ( 'NONE',  ( 229.5999999999999375, -34.91249999999999432, 101.7320508075688821 ) ) ;
#13567 = CARTESIAN_POINT ( 'NONE',  ( 232.5999999999999375, -29.99999999999999645, -47.00000000000010658 ) ) ;
#13568 = VERTEX_POINT ( 'NONE', #2174 ) ;
#13569 = CARTESIAN_POINT ( 'NONE',  ( -4.000000000000000000, 0.9868501483902560878, -0.09357334158579519445 ) ) ;
#13570 = CARTESIAN_POINT ( 'NONE',  ( -6.473970235329672780E-16, -4.862606272033106691, -3.745885042887442395 ) ) ;
#13571 =( GEOMETRIC_REPRESENTATION_CONTEXT ( 3 ) GLOBAL_UNCERTAINTY_ASSIGNED_CONTEXT ( ( #13588 ) ) GLOBAL_UNIT_ASSIGNED_CONTEXT ( ( #14363, #8315, #9689 ) ) REPRESENTATION_CONTEXT ( 'NONE', 'WORKASPACE' ) );
#13572 = CARTESIAN_POINT ( 'NONE',  ( -85.15643035624999868, -34.26562499938548711, 101.5914258081833879 ) ) ;
#13573 = CARTESIAN_POINT ( 'NONE',  ( -85.40000000000000568, -34.50000000000000000, 99.99999999999998579 ) ) ;
#13574 = EDGE_CURVE ( 'NONE', #17308, #6543, #8131, .T. ) ;
#13575 = CARTESIAN_POINT ( 'NONE',  ( -80.90000000000000568, -31.14374999877097139, 102.5980762113533018 ) ) ;
#13576 = CARTESIAN_POINT ( 'NONE',  ( 231.7961524227065695, -33.69240381056765443, 96.99999999999998579 ) ) ;
#13577 = CARTESIAN_POINT ( 'NONE',  ( 109.9999999999999858, -1.526556658859589991E-13, -2.648153673532450419E-29 ) ) ;
#13578 = FACE_OUTER_BOUND ( 'NONE', #17321, .T. ) ;
#13579 = CARTESIAN_POINT ( 'NONE',  ( 4.158921614371309694, 4.076055977742305103, -0.05993604794450720780 ) ) ;
#13580 = CARTESIAN_POINT ( 'NONE',  ( -80.85389467647067363, -35.00000000000000000, -102.4890844034573831 ) ) ;
#13581 = CARTESIAN_POINT ( 'NONE',  ( 235.3564303562499447, -32.12812499938547717, 98.40857419181659793 ) ) ;
#13582 = ORIENTED_EDGE ( 'NONE', *, *, #8517, .T. ) ;
#13583 = CARTESIAN_POINT ( 'NONE',  ( -81.02178482187500208, -32.99062499938548854, -102.3871387122750889 ) ) ;
#13584 = CARTESIAN_POINT ( 'NONE',  ( -82.40000000000000568, -30.00000000000000355, 99.99999999999998579 ) ) ;
#13585 = CARTESIAN_POINT ( 'NONE',  ( 232.5999999999999375, -33.71249999999999147, 96.99999999999998579 ) ) ;
#13586 = DIRECTION ( 'NONE',  ( -0.000000000000000000, -1.000000000000000000, -0.000000000000000000 ) ) ;
#13587 = DIRECTION ( 'NONE',  ( -0.000000000000000000, -1.000000000000000000, -0.000000000000000000 ) ) ;
#13588 = UNCERTAINTY_MEASURE_WITH_UNIT (LENGTH_MEASURE( 1.000000000000000082E-05 ), #14363, 'distance_accuracy_value', 'NONE');
#13589 = CARTESIAN_POINT ( 'NONE',  ( 229.8435696437499871, -35.05312499938547433, -48.40857419181671162 ) ) ;
#13590 = ORIENTED_EDGE ( 'NONE', *, *, #17160, .T. ) ;
#13591 = ORIENTED_EDGE ( 'NONE', *, *, #3143, .F. ) ;
#13592 = CARTESIAN_POINT ( 'NONE',  ( -82.86160995759654213, -32.00000000000002132, 102.8104067583495578 ) ) ;
#13593 = CARTESIAN_POINT ( 'NONE',  ( -85.40000000000000568, -30.90000000000000213, 99.99999999999998579 ) ) ;
#13594 = CARTESIAN_POINT ( 'NONE',  ( -83.90000000000000568, -32.56874999877096855, 102.5980762113533018 ) ) ;
#13595 = CARTESIAN_POINT ( 'NONE',  ( 79.39999999999999147, -31.61250000000000071, 98.26794919243113213 ) ) ;
#13596 = CARTESIAN_POINT ( 'NONE',  ( 82.39999999999999147, -33.43124999877097281, 96.99999999999998579 ) ) ;
#13597 = CARTESIAN_POINT ( 'NONE',  ( 235.3564303562499447, -33.06562499938547717, 99.99999999999998579 ) ) ;
#13598 = CIRCLE ( 'NONE', #2680, 2.199999999999993516 ) ;
#13599 = CARTESIAN_POINT ( 'NONE',  ( 232.5999999999999943, -34.75312499938547717, -53.18285161636690361 ) ) ;
#13600 = CARTESIAN_POINT ( 'NONE',  ( 79.79868554276785630, -32.00000000000000000, -98.52838665788617334 ) ) ;
#13601 = CARTESIAN_POINT ( 'NONE',  ( 81.02178482187500208, -33.59062499938548285, -102.3871387122750889 ) ) ;
#13602 = ORIENTED_EDGE ( 'NONE', *, *, #2774, .F. ) ;
#13603 = CARTESIAN_POINT ( 'NONE',  ( 235.5999999999999943, -33.33749999999999147, -51.73205080756900287 ) ) ;
#13604 = CARTESIAN_POINT ( 'NONE',  ( 83.90000000000000568, -34.87500000000000000, -102.5980762113533018 ) ) ;
#13605 = CARTESIAN_POINT ( 'NONE',  ( 79.64356964375001269, -33.55312499938548854, -101.5914258081833879 ) ) ;
#13606 = AXIS2_PLACEMENT_3D ( 'NONE', #13844, #3205, #4787 ) ;
#13607 = DIRECTION ( 'NONE',  ( -0.000000000000000000, -1.000000000000000000, -0.000000000000000000 ) ) ;
#13608 = CARTESIAN_POINT ( 'NONE',  ( -85.15643035624999868, -30.74062499938548143, 98.40857419181659793 ) ) ;
#13609 = CARTESIAN_POINT ( 'NONE',  ( 229.8435696437499871, -32.91562499938547859, -48.40857419181671162 ) ) ;
#13610 = CARTESIAN_POINT ( 'NONE',  ( -79.39999999999999147, -30.67500000000000071, 99.99999999999998579 ) ) ;
#13611 = ORIENTED_EDGE ( 'NONE', *, *, #3262, .T. ) ;
#13612 = CARTESIAN_POINT ( 'NONE',  ( -82.67676497412369940, -35.00026477264749047, 103.0072806454569303 ) ) ;
#13613 =( BOUNDED_CURVE ( )  B_SPLINE_CURVE ( 2, ( #15426, #6351, #6641, #18556, #14054, #5081, #12303, #688, #4887 ),
 .UNSPECIFIED., .F., .F. ) 
 B_SPLINE_CURVE_WITH_KNOTS ( ( 3, 2, 2, 2, 3 ),
 ( 0.3958333333333334259, 0.4027777777777777901, 0.4166666666666666852, 0.4305555555555555802, 0.4375000000000000555 ),
 .UNSPECIFIED. ) 
 CURVE ( )  GEOMETRIC_REPRESENTATION_ITEM ( )  RATIONAL_B_SPLINE_CURVE ( ( 0.9330127018922192983, 0.9330127018922200755, 1.000000000000000000, 0.8660254037844387076, 1.000000000000000000, 0.8660254037844387076, 1.000000000000000000, 0.9330127018922187432, 0.9330127018922192983 ) ) 
 REPRESENTATION_ITEM ( '' )  );
#13614 = DIRECTION ( 'NONE',  ( -0.000000000000000000, -1.000000000000000000, -0.000000000000000000 ) ) ;
#13615 = CARTESIAN_POINT ( 'NONE',  ( 230.5523683116323355, -32.00000000000000000, 101.8452947671440540 ) ) ;
#13616 = CARTESIAN_POINT ( 'NONE',  ( -82.39999999999999147, -33.70856250001228460, 96.53589838486223584 ) ) ;
#13617 = CARTESIAN_POINT ( 'NONE',  ( 232.5999999999999375, -34.86562499938548143, -53.18285161636690361 ) ) ;
#13618 = CARTESIAN_POINT ( 'NONE',  ( 1.654252653721905331, 3.663718938583014229, -0.01223254789873410957 ) ) ;
#13619 = CARTESIAN_POINT ( 'NONE',  ( -79.64356964374999848, -30.47812499938548569, 99.99999999999998579 ) ) ;
#13620 = CIRCLE ( 'NONE', #1158, 6.000000000000005329 ) ;
#13621 = CARTESIAN_POINT ( 'NONE',  ( 229.9986727058461611, -34.99999999999999289, 101.2112556744905874 ) ) ;
#13622 = CARTESIAN_POINT ( 'NONE',  ( 85.15643035624999868, -35.16562499938547859, 98.40857419181659793 ) ) ;
#13623 = CARTESIAN_POINT ( 'NONE',  ( -85.40000000000000568, -32.73750000000000426, 98.26794919243111792 ) ) ;
#13624 = CARTESIAN_POINT ( 'NONE',  ( 235.3564303562499447, -31.22812499938548214, -51.59142580818350865 ) ) ;
#13625 = CARTESIAN_POINT ( 'NONE',  ( -81.02178482187500208, -32.20312499938548711, 97.61286128772489690 ) ) ;
#13626 = CARTESIAN_POINT ( 'NONE',  ( -82.39999999999999147, -33.96562499938548285, -103.1828516163667899 ) ) ;
#13627 = ORIENTED_EDGE ( 'NONE', *, *, #16494, .T. ) ;
#13628 = CARTESIAN_POINT ( 'NONE',  ( 81.02178482187500208, -31.30312499938548498, 102.3871387122750889 ) ) ;
#13629 = CARTESIAN_POINT ( 'NONE',  ( 105.1999999999999744, -31.99999999999999289, 153.0000000000000000 ) ) ;
#13630 = EDGE_CURVE ( 'NONE', #13743, #18412, #71, .T. ) ;
#13631 = LINE ( 'NONE', #9048, #11456 ) ;
#13632 = CARTESIAN_POINT ( 'NONE',  ( -82.39999999999999147, -32.61562499938548854, 96.81714838363319586 ) ) ;
#13633 = DIRECTION ( 'NONE',  ( -0.000000000000000000, -1.000000000000000000, -0.000000000000000000 ) ) ;
#13634 = EDGE_LOOP ( 'NONE', ( #7611, #1863, #3696, #6283 ) ) ;
#13635 = CARTESIAN_POINT ( 'NONE',  ( -85.40000000000000568, -31.80000000000000071, -99.99999999999998579 ) ) ;
#13636 = AXIS2_PLACEMENT_3D ( 'NONE', #18448, #483, #3688 ) ;
#13637 = EDGE_CURVE ( 'NONE', #5607, #4516, #11350, .T. ) ;
#13638 =( GEOMETRIC_REPRESENTATION_CONTEXT ( 3 ) GLOBAL_UNCERTAINTY_ASSIGNED_CONTEXT ( ( #5114 ) ) GLOBAL_UNIT_ASSIGNED_CONTEXT ( ( #17999, #12026, #14960 ) ) REPRESENTATION_CONTEXT ( 'NONE', 'WORKASPACE' ) );
#13639 = EDGE_CURVE ( 'NONE', #893, #15550, #1369, .T. ) ;
#13640 = CARTESIAN_POINT ( 'NONE',  ( 83.60689295392862164, -35.00000000000000000, 102.7535308243271288 ) ) ;
#13641 = DIRECTION ( 'NONE',  ( -0.000000000000000000, -0.000000000000000000, -1.000000000000000000 ) ) ;
#13642 = CARTESIAN_POINT ( 'NONE',  ( -79.64356964375001269, -32.31562499938548427, -98.40857419181659793 ) ) ;
#13643 = CARTESIAN_POINT ( 'NONE',  ( -0.6810597143197697489, -4.461075778259609770, -3.598441714920717516 ) ) ;
#13644 = CARTESIAN_POINT ( 'NONE',  ( 229.8435696437499871, -33.44062499938547717, 98.40857419181659793 ) ) ;
#13645 = CARTESIAN_POINT ( 'NONE',  ( -82.39999999999999147, -31.41018749875868110, 96.53589838486223584 ) ) ;
#13646 = VECTOR ( 'NONE', #1960, 1000.000000000000114 ) ;
#13647 = ORIENTED_EDGE ( 'NONE', *, *, #13574, .T. ) ;
#13648 = CARTESIAN_POINT ( 'NONE',  ( -81.02178482187500208, -33.10312499938548569, 97.61286128772489690 ) ) ;
#13649 = CARTESIAN_POINT ( 'NONE',  ( -83.90000000000000568, -33.46874999877096712, 102.5980762113533018 ) ) ;
#13650 = CARTESIAN_POINT ( 'NONE',  ( 85.15643035625001289, -34.15312499938548285, 98.40857419181659793 ) ) ;
#13651 = CARTESIAN_POINT ( 'NONE',  ( 0.000000000000000000, 0.000000000000000000, 153.0000000000000000 ) ) ;
#13652 = CARTESIAN_POINT ( 'NONE',  ( -82.40000000000001990, -33.88124999877096855, -97.00000000000000000 ) ) ;
#13653 = CARTESIAN_POINT ( 'NONE',  ( 80.90000000000000568, -34.29374999877096997, -102.5980762113533018 ) ) ;
#13654 = VECTOR ( 'NONE', #11509, 1000.000000000000000 ) ;
#13655 = CARTESIAN_POINT ( 'NONE',  ( 231.0999999999999375, -33.97500000000000142, 102.5980762113533018 ) ) ;
#13656 = EDGE_CURVE ( 'NONE', #11864, #2988, #13100, .T. ) ;
#13657 = ORIENTED_EDGE ( 'NONE', *, *, #14228, .T. ) ;
#13658 = CARTESIAN_POINT ( 'NONE',  ( 231.2217848218749339, -32.57812499938548001, -52.38713871227520968 ) ) ;
#13659 = DIRECTION ( 'NONE',  ( 0.000000000000000000, 0.000000000000000000, 1.000000000000000000 ) ) ;
#13660 = CARTESIAN_POINT ( 'NONE',  ( 229.8435696437499303, -30.70312499938548001, 99.99999999999998579 ) ) ;
#13661 = ADVANCED_FACE ( 'NONE', ( #5778 ), #8604, .F. ) ;
#13662 = CARTESIAN_POINT ( 'NONE',  ( 229.8435696437499871, -30.66562499938547859, -48.40857419181671162 ) ) ;
#13663 = EDGE_CURVE ( 'NONE', #6967, #5568, #7149, .T. ) ;
#13664 = CARTESIAN_POINT ( 'NONE',  ( 4.071447262713887127, 2.020725942163686728, -3.499999999999999556 ) ) ;
#13665 = VECTOR ( 'NONE', #12394, 1000.000000000000000 ) ;
#13666 = ORIENTED_EDGE ( 'NONE', *, *, #8793, .F. ) ;
#13667 = VERTEX_POINT ( 'NONE', #6960 ) ;
#13668 = CARTESIAN_POINT ( 'NONE',  ( -81.02178482187500208, -30.29062499938548569, -102.3871387122750889 ) ) ;
#13669 = CARTESIAN_POINT ( 'NONE',  ( 230.2961164517930968, -35.00002705695778360, 98.07851859032987818 ) ) ;
#13670 = CARTESIAN_POINT ( 'NONE',  ( -80.90000000000000568, -34.80000000000000426, 102.5980762113533018 ) ) ;
#13671 = ORIENTED_EDGE ( 'NONE', *, *, #7675, .F. ) ;
#13672 = FACE_OUTER_BOUND ( 'NONE', #9123, .T. ) ;
#13673 = CYLINDRICAL_SURFACE ( 'NONE', #12365, 5.000000000000000888 ) ;
#13674 = AXIS2_PLACEMENT_3D ( 'NONE', #3685, #18928, #15990 ) ;
#13675 = AXIS2_PLACEMENT_3D ( 'NONE', #10817, #18541, #16784 ) ;
#13676 = CARTESIAN_POINT ( 'NONE',  ( -85.40000000000000568, -30.43124999877096926, 98.26794919243111792 ) ) ;
#13677 = CARTESIAN_POINT ( 'NONE',  ( -79.39999999999999147, -31.51874999877096784, 99.99999999999998579 ) ) ;
#13678 = CARTESIAN_POINT ( 'NONE',  ( -96.99999999999998579, -29.80000000000000426, -150.0000000000000000 ) ) ;
#13679 = CARTESIAN_POINT ( 'NONE',  ( -80.90000000000000568, -33.75000000000000000, 97.40192378864668399 ) ) ;
#13680 = PLANE ( 'NONE',  #10556 ) ;
#13681 = CARTESIAN_POINT ( 'NONE',  ( 3.999999999999999112, -0.7890432684750902093, -0.04868663549882291247 ) ) ;
#13682 = CARTESIAN_POINT ( 'NONE',  ( 229.8435696437499303, -32.39062499938548001, 99.99999999999998579 ) ) ;
#13683 = ORIENTED_EDGE ( 'NONE', *, *, #8266, .F. ) ;
#13684 = CARTESIAN_POINT ( 'NONE',  ( -81.02178482187500208, -33.44062499938548427, -102.3871387122750889 ) ) ;
#13685 = CARTESIAN_POINT ( 'NONE',  ( 105.1999999999999744, -29.80000000000000071, 150.0000000000000000 ) ) ;
#13686 = AXIS2_PLACEMENT_3D ( 'NONE', #14956, #3224, #1580 ) ;
#13687 = ORIENTED_EDGE ( 'NONE', *, *, #10541, .F. ) ;
#13688 = EDGE_CURVE ( 'NONE', #6735, #7760, #19071, .T. ) ;
#13689 = CARTESIAN_POINT ( 'NONE',  ( -83.20384757729338787, -33.63615380933863719, 97.00000000000000000 ) ) ;
#13690 = CARTESIAN_POINT ( 'NONE',  ( 231.7961524227065695, -34.53615380933862866, 96.99999999999998579 ) ) ;
#13691 = CARTESIAN_POINT ( 'NONE',  ( 229.6880761451917579, -35.00000000000001421, -50.39325454734051846 ) ) ;
#13692 = EDGE_CURVE ( 'NONE', #2826, #2762, #8910, .T. ) ;
#13693 = B_SPLINE_CURVE_WITH_KNOTS ( 'NONE', 3,
 ( #470, #10618, #376, #8702, #13640, #10713, #18244, #12374, #12180, #7329 ),
 .UNSPECIFIED., .F., .F.,
 ( 4, 2, 2, 2, 4 ),
 ( 0.3612006186103786654, 0.3925526867148934063, 0.4239047548194081472, 0.4552568229239228881, 0.4866088910284376290 ),
 .UNSPECIFIED. ) ;
#13694 = FACE_OUTER_BOUND ( 'NONE', #18347, .T. ) ;
#13695 = ORIENTED_EDGE ( 'NONE', *, *, #1401, .T. ) ;
#13696 = VERTEX_POINT ( 'NONE', #2544 ) ;
#13697 = FACE_OUTER_BOUND ( 'NONE', #1181, .T. ) ;
#13698 = CARTESIAN_POINT ( 'NONE',  ( 83.90000000000000568, -30.97500000000000142, -97.40192378864668399 ) ) ;
#13699 = CARTESIAN_POINT ( 'NONE',  ( -83.90000000000000568, -33.16874999877096286, 97.40192378864668399 ) ) ;
#13700 = CARTESIAN_POINT ( 'NONE',  ( 85.40000000000000568, -31.83750000000000568, 101.7320508075688679 ) ) ;
#13701 = EDGE_CURVE ( 'NONE', #6061, #4621, #8506, .T. ) ;
#13702 = CARTESIAN_POINT ( 'NONE',  ( -82.39999999999999147, -32.81250000000000000, 97.00000000000000000 ) ) ;
#13703 = CARTESIAN_POINT ( 'NONE',  ( 231.2217848218749339, -34.26562499938548001, 97.61286128772489690 ) ) ;
#13704 = CARTESIAN_POINT ( 'NONE',  ( 79.64356964374998427, -34.11562499938548854, -101.5914258081833879 ) ) ;
#13705 = CYLINDRICAL_SURFACE ( 'NONE', #1523, 3.000000000000002665 ) ;
#13706 = CARTESIAN_POINT ( 'NONE',  ( 81.02178482187500208, -33.14062499938548711, -102.3871387122750889 ) ) ;
#13707 = ORIENTED_EDGE ( 'NONE', *, *, #18906, .T. ) ;
#13708 = CARTESIAN_POINT ( 'NONE',  ( 235.5999999999999943, -32.96249999999999858, -48.26794919243124582 ) ) ;
#13709 = CARTESIAN_POINT ( 'NONE',  ( 82.39999999999999147, -32.27812499938548285, -103.1828516163667899 ) ) ;
#13710 = CARTESIAN_POINT ( 'NONE',  ( 85.15643035624999868, -33.70312499938548711, -101.5914258081833879 ) ) ;
#13711 = CARTESIAN_POINT ( 'NONE',  ( 0.000000000000000000, 0.000000000000000000, 0.000000000000000000 ) ) ;
#13712 = CARTESIAN_POINT ( 'NONE',  ( -82.39999999999999147, -31.49062499938548854, 103.1828516163667899 ) ) ;
#13713 = CARTESIAN_POINT ( 'NONE',  ( 229.8435696437499871, -32.09062499938548285, -51.59142580818350865 ) ) ;
#13714 = CARTESIAN_POINT ( 'NONE',  ( -85.40000000000000568, -30.90000000000000213, 99.99999999999998579 ) ) ;
#13715 = ORIENTED_EDGE ( 'NONE', *, *, #14490, .F. ) ;
#13716 = CARTESIAN_POINT ( 'NONE',  ( -79.60928765286361397, -35.00091442770696659, 98.84622810931887216 ) ) ;
#13717 = CARTESIAN_POINT ( 'NONE',  ( 235.3564303562499447, -34.00312499938547717, 101.5914258081833879 ) ) ;
#13718 = CARTESIAN_POINT ( 'NONE',  ( 81.02178482187500208, -30.74062499938548498, 102.3871387122750889 ) ) ;
#13719 = CARTESIAN_POINT ( 'NONE',  ( 85.40000000000000568, -32.64374999877097139, -99.99999999999998579 ) ) ;
#13720 = CARTESIAN_POINT ( 'NONE',  ( -82.39999999999999147, -30.59062499938548640, 103.1828516163667899 ) ) ;
#13721 = CARTESIAN_POINT ( 'NONE',  ( 230.4006479041920272, -35.00000000000000000, 101.7928000422452897 ) ) ;
#13722 = CARTESIAN_POINT ( 'NONE',  ( 79.64356964375001269, -30.77812499938548285, 101.5914258081833879 ) ) ;
#13723 = CARTESIAN_POINT ( 'NONE',  ( 79.64356964375001269, -32.24062499938548854, -98.40857419181659793 ) ) ;
#13724 = CARTESIAN_POINT ( 'NONE',  ( 233.9782151781249411, -30.29062499938547859, -52.38713871227520968 ) ) ;
#13725 = CARTESIAN_POINT ( 'NONE',  ( -84.56803305035340657, -32.00000000000000000, -98.28830862702052684 ) ) ;
#13726 = CARTESIAN_POINT ( 'NONE',  ( -79.64356964375001269, -33.59062499938548285, -101.5914258081833879 ) ) ;
#13727 = PRODUCT_DEFINITION_CONTEXT ( 'detailed design', #6962, 'design' ) ;
#13728 = VERTEX_POINT ( 'NONE', #7048 ) ;
#13729 = CARTESIAN_POINT ( 'NONE',  ( 83.90000000000000568, -34.81874999877096855, 97.40192378864668399 ) ) ;
#13730 = EDGE_CURVE ( 'NONE', #14449, #10754, #5987, .T. ) ;
#13731 = CARTESIAN_POINT ( 'NONE',  ( 234.0999999999999375, -34.19999999999999574, 97.40192378864668399 ) ) ;
#13732 = CARTESIAN_POINT ( 'NONE',  ( 4.071447262713888016, -2.020725942163695166, -3.500000000000000000 ) ) ;
#13733 = CARTESIAN_POINT ( 'NONE',  ( -82.39999999999999147, -32.84062499938548996, 103.1828516163667899 ) ) ;
#13734 = DIRECTION ( 'NONE',  ( -1.000000000000000000, -0.000000000000000000, -0.000000000000000000 ) ) ;
#13735 = ORIENTED_EDGE ( 'NONE', *, *, #17157, .F. ) ;
#13736 = CARTESIAN_POINT ( 'NONE',  ( -83.25523545990762386, -35.19352049914630953, -103.2690260512239604 ) ) ;
#13737 = CARTESIAN_POINT ( 'NONE',  ( 83.33080762004576059, -35.05289549976084373, -96.44210921874548603 ) ) ;
#13738 = CARTESIAN_POINT ( 'NONE',  ( 81.59615242270665192, -33.67634618820330417, 103.0000000000000000 ) ) ;
#13739 = CARTESIAN_POINT ( 'NONE',  ( 82.40000000000000568, -33.71249999999998437, 102.9999999999999858 ) ) ;
#13740 = CARTESIAN_POINT ( 'NONE',  ( -82.40000000000000568, -35.00000000000000000, 92.49999999999997158 ) ) ;
#13741 = CARTESIAN_POINT ( 'NONE',  ( 235.3564303562499447, -34.11562499938548143, 101.5914258081833879 ) ) ;
#13742 = CARTESIAN_POINT ( 'NONE',  ( -82.39999999999999147, -32.08518749875868536, 103.4641016151377499 ) ) ;
#13743 = VERTEX_POINT ( 'NONE', #14656 ) ;
#13744 = DIRECTION ( 'NONE',  ( 0.2773500981126160725, 0.4803844614152618653, 0.8320502943378429439 ) ) ;
#13745 = CARTESIAN_POINT ( 'NONE',  ( -83.20384757729335945, -33.63615380933863008, 96.99999999999998579 ) ) ;
#13746 = CARTESIAN_POINT ( 'NONE',  ( 85.15643035625001289, -32.42812499938548854, 101.5914258081833879 ) ) ;
#13747 = LINE ( 'NONE', #385, #5265 ) ;
#13748 = DIRECTION ( 'NONE',  ( 0.000000000000000000, 0.000000000000000000, -1.000000000000000000 ) ) ;
#13749 = CARTESIAN_POINT ( 'NONE',  ( 82.39999999999999147, -34.10624999877096997, -96.53589838486223584 ) ) ;
#13750 = CARTESIAN_POINT ( 'NONE',  ( 25.60000000000000142, 0.000000000000000000, 0.000000000000000000 ) ) ;
#13751 = ADVANCED_FACE ( 'NONE', ( #4313 ), #6612, .T. ) ;
#13752 = VERTEX_POINT ( 'NONE', #9345 ) ;
#13753 = CARTESIAN_POINT ( 'NONE',  ( 231.2217848218749339, -32.87812499938547717, -47.61286128772501769 ) ) ;
#13754 = DIRECTION ( 'NONE',  ( 1.000000000000000000, 0.000000000000000000, 0.000000000000000000 ) ) ;
#13755 = CARTESIAN_POINT ( 'NONE',  ( 231.2217848218749339, -32.87812499938547717, 102.3871387122750889 ) ) ;
#13756 = CARTESIAN_POINT ( 'NONE',  ( 231.2217848218749339, -30.32812499938548001, -52.38713871227520968 ) ) ;
#13757 = CARTESIAN_POINT ( 'NONE',  ( -81.59615242270662350, -32.83259618943233704, -102.9999999999999716 ) ) ;
#13758 = VERTEX_POINT ( 'NONE', #9249 ) ;
#13759 = ORIENTED_EDGE ( 'NONE', *, *, #18906, .F. ) ;
#13760 = CARTESIAN_POINT ( 'NONE',  ( -82.14831453752226764, -31.99999999999999289, 97.14155664245926403 ) ) ;
#13761 = CARTESIAN_POINT ( 'NONE',  ( -79.39999999999999147, -33.73124999877096997, -101.7320508075688963 ) ) ;
#13762 = FACE_OUTER_BOUND ( 'NONE', #9826, .T. ) ;
#13763 = ORIENTED_EDGE ( 'NONE', *, *, #14490, .T. ) ;
#13764 = ADVANCED_FACE ( 'NONE', ( #6239 ), #14035, .T. ) ;
#13765 = CARTESIAN_POINT ( 'NONE',  ( 85.15643035625001289, -32.05312499938548854, 99.99999999999998579 ) ) ;
#13766 = CARTESIAN_POINT ( 'NONE',  ( -85.40000000000000568, -33.58124999877097139, -101.7320508075688679 ) ) ;
#13767 = ADVANCED_FACE ( 'NONE', ( #8082 ), #7979, .F. ) ;
#13768 = CARTESIAN_POINT ( 'NONE',  ( -80.90000000000000568, -33.89999999999999858, 102.5980762113533018 ) ) ;
#13769 = CARTESIAN_POINT ( 'NONE',  ( -83.90000000000000568, -30.91874999877096997, 97.40192378864668399 ) ) ;
#13770 = CARTESIAN_POINT ( 'NONE',  ( -85.40000000000000568, -34.85624999877096997, 101.7320508075688679 ) ) ;
#13771 = CARTESIAN_POINT ( 'NONE',  ( -82.40000000000001990, -32.08124999877097139, 103.0000000000000000 ) ) ;
#13772 = CARTESIAN_POINT ( 'NONE',  ( -82.40000000000000568, -33.93750000000000711, 102.9999999999999858 ) ) ;
#13773 = CARTESIAN_POINT ( 'NONE',  ( 79.39999999999999147, -34.72500000000000142, -99.99999999999998579 ) ) ;
#13774 = DIRECTION ( 'NONE',  ( 0.000000000000000000, 0.000000000000000000, 1.000000000000000000 ) ) ;
#13775 = CARTESIAN_POINT ( 'NONE',  ( 229.8435696437499871, -35.05312499938547433, 101.5914258081833879 ) ) ;
#13776 = EDGE_CURVE ( 'NONE', #7903, #10919, #5061, .T. ) ;
#13777 = CARTESIAN_POINT ( 'NONE',  ( 232.5999999999999375, -32.72812499938547859, 103.1828516163667899 ) ) ;
#13778 = EDGE_LOOP ( 'NONE', ( #7106, #12128, #18212, #16093 ) ) ;
#13779 = CARTESIAN_POINT ( 'NONE',  ( -83.77821517812500929, -32.46562499938548285, -102.3871387122750889 ) ) ;
#13780 = CARTESIAN_POINT ( 'NONE',  ( 99.99999999999997158, -31.99999999999999289, -100.0000000000000000 ) ) ;
#13781 = ORIENTED_EDGE ( 'NONE', *, *, #5603, .T. ) ;
#13782 = CARTESIAN_POINT ( 'NONE',  ( 110.0000000000000142, 10.19999999999997620, -130.0000000000000000 ) ) ;
#13783 = FACE_OUTER_BOUND ( 'NONE', #6449, .T. ) ;
#13784 = CARTESIAN_POINT ( 'NONE',  ( 230.2491162085310066, -35.00000000000002132, -48.39201219457986980 ) ) ;
#13785 = ORIENTED_EDGE ( 'NONE', *, *, #7470, .F. ) ;
#13786 = DIRECTION ( 'NONE',  ( 0.000000000000000000, 0.000000000000000000, 1.000000000000000000 ) ) ;
#13787 = TOROIDAL_SURFACE ( 'NONE', #12542, 5.200000000000001066, 0.4999999999999978351 ) ;
#13788 = ORIENTED_EDGE ( 'NONE', *, *, #10678, .F. ) ;
#13789 = ORIENTED_EDGE ( 'NONE', *, *, #16365, .T. ) ;
#13790 = CARTESIAN_POINT ( 'NONE',  ( 82.39999999999999147, -30.11250000000000426, -96.53589838486223584 ) ) ;
#13791 = CARTESIAN_POINT ( 'NONE',  ( -83.90000000000000568, -33.46874999877096712, 102.5980762113533018 ) ) ;
#13792 = CARTESIAN_POINT ( 'NONE',  ( -83.74167325096722436, -32.00000000000001421, -97.53412486788926117 ) ) ;
#13793 = CARTESIAN_POINT ( 'NONE',  ( 235.3564303562499447, -33.96562499938547575, 99.99999999999998579 ) ) ;
#13794 = CARTESIAN_POINT ( 'NONE',  ( 85.15643035625001289, -33.89062499938548711, -98.40857419181659793 ) ) ;
#13795 = CARTESIAN_POINT ( 'NONE',  ( 83.92761994968586237, -31.99999999999999289, -97.66884955413871694 ) ) ;
#13796 = AXIS2_PLACEMENT_3D ( 'NONE', #13711, #1611, #13425 ) ;
#13797 = CARTESIAN_POINT ( 'NONE',  ( 85.15643035625001289, -34.64062499938548711, -99.99999999999998579 ) ) ;
#13798 = ORIENTED_EDGE ( 'NONE', *, *, #2844, .F. ) ;
#13799 = CARTESIAN_POINT ( 'NONE',  ( 235.5999999999999943, -32.43749999999999289, -51.73205080756900287 ) ) ;
#13800 = CARTESIAN_POINT ( 'NONE',  ( -82.39999999999999147, -34.61250000000000426, 96.53589838486223584 ) ) ;
#13801 = CARTESIAN_POINT ( 'NONE',  ( 82.40000000000000568, -33.43124999877096570, -102.9999999999999858 ) ) ;
#13802 = CARTESIAN_POINT ( 'NONE',  ( 229.5999999999999091, -34.97364041986482164, -51.09190422181774949 ) ) ;
#13803 = CARTESIAN_POINT ( 'NONE',  ( -83.77821517812500929, -32.12812499938548427, 97.61286128772489690 ) ) ;
#13804 = EDGE_CURVE ( 'NONE', #4300, #4443, #260, .T. ) ;
#13805 = CARTESIAN_POINT ( 'NONE',  ( 235.3564303562499447, -34.04062499938547859, -51.59142580818350865 ) ) ;
#13806 = CARTESIAN_POINT ( 'NONE',  ( -82.39999999999999147, -33.03750000000000142, 103.4641016151377499 ) ) ;
#13807 = VERTEX_POINT ( 'NONE', #3394 ) ;
#13808 = CARTESIAN_POINT ( 'NONE',  ( -80.85786485831481230, -34.99991206035976887, 102.5785900675527813 ) ) ;
#13809 = CIRCLE ( 'NONE', #3522, 4.000000000000000000 ) ;
#13810 = CYLINDRICAL_SURFACE ( 'NONE', #4780, 3.000000000000009770 ) ;
#13811 = CARTESIAN_POINT ( 'NONE',  ( 5.384454397937118664, 0.000000000000000000, -5.000000000000000000 ) ) ;
#13812 = CARTESIAN_POINT ( 'NONE',  ( 85.12124608221321864, -32.00000000000000000, -99.52644304242026863 ) ) ;
#13813 = CARTESIAN_POINT ( 'NONE',  ( -85.15643035625001289, -32.50312499938548427, 99.99999999999998579 ) ) ;
#13814 = CARTESIAN_POINT ( 'NONE',  ( 83.77821517812500929, -34.22812499938549280, 97.61286128772489690 ) ) ;
#13815 = CARTESIAN_POINT ( 'NONE',  ( 82.39999999999999147, -30.59062499938548640, -103.1828516163667899 ) ) ;
#13816 = CARTESIAN_POINT ( 'NONE',  ( 231.2217848218749339, -31.86562499938547788, -47.61286128772501769 ) ) ;
#13817 = CARTESIAN_POINT ( 'NONE',  ( -81.02178482187500208, -32.09062499938548285, 97.61286128772489690 ) ) ;
#13818 = CARTESIAN_POINT ( 'NONE',  ( -82.39999999999999147, -34.19062499938548427, -96.81714838363319586 ) ) ;
#13819 = AXIS2_PLACEMENT_3D ( 'NONE', #10860, #10664, #3334 ) ;
#13820 = ORIENTED_EDGE ( 'NONE', *, *, #16453, .T. ) ;
#13821 = CARTESIAN_POINT ( 'NONE',  ( 83.77821517812500929, -33.02812499938548285, 102.3871387122750889 ) ) ;
#13822 = CARTESIAN_POINT ( 'NONE',  ( 232.5999999999999659, -32.13749999999999574, 102.9999999999999858 ) ) ;
#13823 = CARTESIAN_POINT ( 'NONE',  ( 4.175326769692872197, -2.060699556488933215, -3.569236330973462490 ) ) ;
#13824 = CARTESIAN_POINT ( 'NONE',  ( -79.64356964375001269, -33.59062499938548285, 98.40857419181659793 ) ) ;
#13825 = DIRECTION ( 'NONE',  ( -0.000000000000000000, -1.000000000000000000, -0.000000000000000000 ) ) ;
#13826 = ORIENTED_EDGE ( 'NONE', *, *, #17471, .F. ) ;
#13827 = CARTESIAN_POINT ( 'NONE',  ( -82.39999999999999147, -30.78750000000000497, -96.53589838486223584 ) ) ;
#13828 = CARTESIAN_POINT ( 'NONE',  ( 85.40000000000000568, -34.95000000000000284, -99.99999999999998579 ) ) ;
#13829 = CARTESIAN_POINT ( 'NONE',  ( -83.32052461991715120, -34.98323688327303671, -102.9326364780328760 ) ) ;
#13830 = FACE_OUTER_BOUND ( 'NONE', #2412, .T. ) ;
#13831 = CARTESIAN_POINT ( 'NONE',  ( 235.5999999999999943, -32.83124999877096428, -51.73205080756900287 ) ) ;
#13832 = CARTESIAN_POINT ( 'NONE',  ( 229.8435696437499871, -35.16562499938547148, 101.5914258081833879 ) ) ;
#13833 = CARTESIAN_POINT ( 'NONE',  ( -85.40000000000000568, -33.51018749875867542, 101.7320508075688679 ) ) ;
#13834 = ORIENTED_EDGE ( 'NONE', *, *, #8150, .F. ) ;
#13835 = CARTESIAN_POINT ( 'NONE',  ( 232.5999999999999659, -32.81249999999999289, 97.00000000000000000 ) ) ;
#13836 = CARTESIAN_POINT ( 'NONE',  ( 85.40000000000000568, -34.53750000000000142, -98.26794919243111792 ) ) ;
#13837 = CARTESIAN_POINT ( 'NONE',  ( 230.1700715539191435, -32.00000000000000000, 98.68659295968620881 ) ) ;
#13838 = CARTESIAN_POINT ( 'NONE',  ( 82.40000000000001990, -32.08124999877097139, -103.0000000000000000 ) ) ;
#13839 = FACE_OUTER_BOUND ( 'NONE', #4719, .T. ) ;
#13840 = CARTESIAN_POINT ( 'NONE',  ( 85.15643035624999868, -31.64062499938548356, -98.40857419181659793 ) ) ;
#13841 = CARTESIAN_POINT ( 'NONE',  ( 232.5999999999999375, -29.99999999999999645, -53.00000000000012079 ) ) ;
#13842 = ORIENTED_EDGE ( 'NONE', *, *, #10207, .T. ) ;
#13843 = CARTESIAN_POINT ( 'NONE',  ( 232.5999999999999943, -33.06562499938547717, -53.18285161636690361 ) ) ;
#13844 = CARTESIAN_POINT ( 'NONE',  ( 0.000000000000000000, 0.000000000000000000, 0.000000000000000000 ) ) ;
#13845 = CARTESIAN_POINT ( 'NONE',  ( 233.9782151781249411, -32.80312499938548143, 102.3871387122750889 ) ) ;
#13846 = CARTESIAN_POINT ( 'NONE',  ( 230.3018604581529871, -35.39427337414328889, -51.92835542527824089 ) ) ;
#13847 = CARTESIAN_POINT ( 'NONE',  ( -85.15643035625001289, -33.74062499938548854, 99.99999999999998579 ) ) ;
#13848 = CARTESIAN_POINT ( 'NONE',  ( 233.4038475772933339, -34.81740381056766154, -47.00000000000011369 ) ) ;
#13849 = ORIENTED_EDGE ( 'NONE', *, *, #14158, .F. ) ;
#13850 = ORIENTED_EDGE ( 'NONE', *, *, #4155, .T. ) ;
#13851 = CARTESIAN_POINT ( 'NONE',  ( 4.211140560182196957, -2.431303136016555122, -3.745885042887436622 ) ) ;
#13852 = CARTESIAN_POINT ( 'NONE',  ( -79.39999999999999147, -33.76874999877097139, -99.99999999999998579 ) ) ;
#13853 = CARTESIAN_POINT ( 'NONE',  ( 4.158413352280811104, -4.089743253945655077, 5.067843131179045271E-16 ) ) ;
#13854 = VERTEX_POINT ( 'NONE', #15308 ) ;
#13855 = CARTESIAN_POINT ( 'NONE',  ( -2.500000000000000444, 3.061616997868383634E-16, -25.03750572909317285 ) ) ;
#13856 = CARTESIAN_POINT ( 'NONE',  ( -80.90000000000000568, -33.24374999877097281, -102.5980762113533018 ) ) ;
#13857 = CARTESIAN_POINT ( 'NONE',  ( -79.39999999999999147, -33.78750000000000853, 98.26794919243110371 ) ) ;
#13858 = CARTESIAN_POINT ( 'NONE',  ( -85.40000000000000568, -32.15624999877096712, 101.7320508075688679 ) ) ;
#13859 = CARTESIAN_POINT ( 'NONE',  ( -79.39999999999999147, -33.28124999877096712, 98.26794919243110371 ) ) ;
#13860 = PRODUCT_DEFINITION_SHAPE ( 'NONE', 'NONE',  #12507 ) ;
#13861 = CARTESIAN_POINT ( 'NONE',  ( 232.5999999999999375, -32.30624999877096570, 97.00000000000000000 ) ) ;
#13862 = CYLINDRICAL_SURFACE ( 'NONE', #10072, 3.000000000000002665 ) ;
#13863 = CARTESIAN_POINT ( 'NONE',  ( 229.5999999999999375, -34.85624999877096286, -48.26794919243123161 ) ) ;
#13864 = CARTESIAN_POINT ( 'NONE',  ( 231.2217848218749339, -33.81562499938547717, 97.61286128772489690 ) ) ;
#13865 = ORIENTED_EDGE ( 'NONE', *, *, #18798, .T. ) ;
#13866 = PRESENTATION_STYLE_ASSIGNMENT (( #3131 ) ) ;
#13867 = CARTESIAN_POINT ( 'NONE',  ( 94.79999999999995453, -5.200000000000000178, -150.0000000000000000 ) ) ;
#13868 = CARTESIAN_POINT ( 'NONE',  ( -69.99999999999998579, -32.00000000000000000, 150.0000000000000000 ) ) ;
#13869 = ORIENTED_EDGE ( 'NONE', *, *, #14250, .F. ) ;
#13870 = DIRECTION ( 'NONE',  ( -1.000000000000000000, 0.000000000000000000, 0.000000000000000000 ) ) ;
#13871 = DIRECTION ( 'NONE',  ( -1.000000000000000000, -0.000000000000000000, -0.000000000000000000 ) ) ;
#13872 = UNCERTAINTY_MEASURE_WITH_UNIT (LENGTH_MEASURE( 1.000000000000000082E-05 ), #7702, 'distance_accuracy_value', 'NONE');
#13873 = CARTESIAN_POINT ( 'NONE',  ( 85.40000000000000568, -33.11250000000000426, -101.7320508075688821 ) ) ;
#13874 = ORIENTED_EDGE ( 'NONE', *, *, #496, .F. ) ;
#13875 = B_SPLINE_CURVE_WITH_KNOTS ( 'NONE', 3,
 ( #11538, #8596, #7142, #1282, #1380, #4401 ),
 .UNSPECIFIED., .F., .F.,
 ( 4, 2, 4 ),
 ( 0.000000000000000000, 0.002086519881787259317, 0.004173039763574518633 ),
 .UNSPECIFIED. ) ;
#13876 = CARTESIAN_POINT ( 'NONE',  ( 229.8435696437499018, -35.11426555956767714, -51.00325860250310939 ) ) ;
#13877 = AXIS2_PLACEMENT_3D ( 'NONE', #12113, #6450, #12401 ) ;
#13878 = VERTEX_POINT ( 'NONE', #17067 ) ;
#13879 = ORIENTED_EDGE ( 'NONE', *, *, #3925, .F. ) ;
#13880 = CARTESIAN_POINT ( 'NONE',  ( 0.000000000000000000, 0.000000000000000000, 0.000000000000000000 ) ) ;
#13881 = CARTESIAN_POINT ( 'NONE',  ( 83.90000000000000568, -31.42500000000000071, -97.40192378864668399 ) ) ;
#13882 = CARTESIAN_POINT ( 'NONE',  ( 4.175813232069147674, -2.061359961916367833, 3.570380186727398542 ) ) ;
#13883 = EDGE_CURVE ( 'NONE', #1498, #4792, #13220, .T. ) ;
#13884 = CARTESIAN_POINT ( 'NONE',  ( -80.90000000000000568, -33.39374999877097139, 102.5980762113533018 ) ) ;
#13885 = CARTESIAN_POINT ( 'NONE',  ( 25.15499999999999758, 3.061616997868383634E-16, -2.500000000000000444 ) ) ;
#13886 = DIRECTION ( 'NONE',  ( 0.000000000000000000, 0.000000000000000000, -1.000000000000000000 ) ) ;
#13887 = CARTESIAN_POINT ( 'NONE',  ( 81.02178482187500208, -33.55312499938548854, -97.61286128772489690 ) ) ;
#13888 = CARTESIAN_POINT ( 'NONE',  ( 84.11496519894586754, -32.00000000000000000, -97.81539907810424950 ) ) ;
#13889 = CARTESIAN_POINT ( 'NONE',  ( -85.15643035624999868, -33.70312499938548711, 101.5914258081833879 ) ) ;
#13890 = VECTOR ( 'NONE', #5148, 1000.000000000000000 ) ;
#13891 = CARTESIAN_POINT ( 'NONE',  ( 79.64356964375001269, -34.37812499938548427, -98.40857419181659793 ) ) ;
#13892 = ORIENTED_EDGE ( 'NONE', *, *, #8892, .F. ) ;
#13893 =( BOUNDED_CURVE ( )  B_SPLINE_CURVE ( 2, ( #8617, #16340, #7251, #4228, #14865, #5791, #7446, #5700, #8715 ),
 .UNSPECIFIED., .F., .F. ) 
 B_SPLINE_CURVE_WITH_KNOTS ( ( 3, 2, 2, 2, 3 ),
 ( 0.7291666666666668517, 0.7361111111111111605, 0.7500000000000000000, 0.7638888888888888395, 0.7708333333333333703 ),
 .UNSPECIFIED. ) 
 CURVE ( )  GEOMETRIC_REPRESENTATION_ITEM ( )  RATIONAL_B_SPLINE_CURVE ( ( 0.9330127018922194093, 0.9330127018922209636, 1.000000000000000000, 0.8660254037844387076, 1.000000000000000000, 0.8660254037844387076, 1.000000000000000000, 0.9330127018922187432, 0.9330127018922192983 ) ) 
 REPRESENTATION_ITEM ( '' )  );
#13894 = CARTESIAN_POINT ( 'NONE',  ( 235.5999999999999943, -31.98749999999999361, -51.73205080756900287 ) ) ;
#13895 = EDGE_CURVE ( 'NONE', #11136, #14354, #5577, .T. ) ;
#13896 = CARTESIAN_POINT ( 'NONE',  ( -85.40000000000000568, -30.93750000000000355, 98.26794919243111792 ) ) ;
#13897 = CARTESIAN_POINT ( 'NONE',  ( 229.8435696437499587, -33.36562499938548143, 101.5914258081833879 ) ) ;
#13898 = CARTESIAN_POINT ( 'NONE',  ( -81.02178482187500208, -32.35312499938548569, 102.3871387122750889 ) ) ;
#13899 = CARTESIAN_POINT ( 'NONE',  ( 233.9782151781249411, -32.80312499938548143, -47.61286128772501769 ) ) ;
#13900 = EDGE_CURVE ( 'NONE', #13349, #11282, #16684, .T. ) ;
#13901 = CARTESIAN_POINT ( 'NONE',  ( -85.40000000000000568, -33.14999999999999858, 99.99999999999998579 ) ) ;
#13902 = ORIENTED_EDGE ( 'NONE', *, *, #1479, .F. ) ;
#13903 = DIRECTION ( 'NONE',  ( 0.000000000000000000, 0.000000000000000000, -1.000000000000000000 ) ) ;
#13904 = VECTOR ( 'NONE', #10027, 1000.000000000000000 ) ;
#13905 = CARTESIAN_POINT ( 'NONE',  ( 80.80861089413670584, -34.99999999999999289, 97.72105564972112290 ) ) ;
#13906 = CARTESIAN_POINT ( 'NONE',  ( 85.15643035625001289, -32.39062499938548711, 99.99999999999998579 ) ) ;
#13907 = CARTESIAN_POINT ( 'NONE',  ( 230.0666556977843697, -31.99999999999998579, -48.89901723339011852 ) ) ;
#13908 = EDGE_CURVE ( 'NONE', #11431, #711, #574, .T. ) ;
#13909 = CARTESIAN_POINT ( 'NONE',  ( -85.15643035625001289, -32.46562499938548996, 101.5914258081833879 ) ) ;
#13910 = CARTESIAN_POINT ( 'NONE',  ( -81.02178482187500208, -32.35312499938548569, -97.61286128772489690 ) ) ;
#13911 = CARTESIAN_POINT ( 'NONE',  ( 82.39999999999999147, -33.96562499938548285, 103.1828516163667899 ) ) ;
#13912 = AXIS2_PLACEMENT_3D ( 'NONE', #6150, #18262, #6250 ) ;
#13913 = CARTESIAN_POINT ( 'NONE',  ( 82.39999999999999147, -31.94062499938548427, -103.1828516163667899 ) ) ;
#13914 = CARTESIAN_POINT ( 'NONE',  ( 235.3564303562499447, -30.77812499938547575, -51.59142580818350865 ) ) ;
#13915 = CARTESIAN_POINT ( 'NONE',  ( -81.02178482187500208, -34.00312499938548427, 97.61286128772489690 ) ) ;
#13916 = CARTESIAN_POINT ( 'NONE',  ( -83.77821517812500929, -33.32812499938548711, -97.61286128772489690 ) ) ;
#13917 = AXIS2_PLACEMENT_3D ( 'NONE', #17553, #4071, #10031 ) ;
#13918 = ORIENTED_EDGE ( 'NONE', *, *, #1592, .F. ) ;
#13919 = CARTESIAN_POINT ( 'NONE',  ( 83.77821517812500929, -33.92812499938548854, 102.3871387122750889 ) ) ;
#13920 = CARTESIAN_POINT ( 'NONE',  ( 4.086262629614029862, -1.979770830881092625, -3.570936333571105070 ) ) ;
#13921 = CARTESIAN_POINT ( 'NONE',  ( -79.64356964375001269, -30.32812499938548711, 98.40857419181659793 ) ) ;
#13922 = CARTESIAN_POINT ( 'NONE',  ( -85.15643035625001289, -34.30312499938548854, 99.99999999999998579 ) ) ;
#13923 =( BOUNDED_CURVE ( )  B_SPLINE_CURVE ( 2, ( #17354, #5451, #15794, #12564, #5352, #11294, #9736, #15699, #17164 ),
 .UNSPECIFIED., .F., .F. ) 
 B_SPLINE_CURVE_WITH_KNOTS ( ( 3, 2, 2, 2, 3 ),
 ( 0.7291666666666667407, 0.7361111111111111605, 0.7500000000000000000, 0.7638888888888888395, 0.7708333333333332593 ),
 .UNSPECIFIED. ) 
 CURVE ( )  GEOMETRIC_REPRESENTATION_ITEM ( )  RATIONAL_B_SPLINE_CURVE ( ( 0.9330127018922192983, 0.9330127018922198534, 1.000000000000000000, 0.8660254037844387076, 1.000000000000000000, 0.8660254037844387076, 1.000000000000000000, 0.9330127018922198534, 0.9330127018922192983 ) ) 
 REPRESENTATION_ITEM ( '' )  );
#13924 = CYLINDRICAL_SURFACE ( 'NONE', #8048, 3.000000000000002665 ) ;
#13925 = ORIENTED_EDGE ( 'NONE', *, *, #11902, .F. ) ;
#13926 = EDGE_CURVE ( 'NONE', #19255, #17445, #10813, .T. ) ;
#13927 = CARTESIAN_POINT ( 'NONE',  ( -83.90000000000000568, -33.22500000000000142, -102.5980762113533018 ) ) ;
#13928 = DIRECTION ( 'NONE',  ( -0.000000000000000000, -1.000000000000000000, -0.000000000000000000 ) ) ;
#13929 = DIRECTION ( 'NONE',  ( -1.000000000000000000, 0.000000000000000000, 0.000000000000000000 ) ) ;
#13930 = DIRECTION ( 'NONE',  ( 0.000000000000000000, 0.000000000000000000, 1.000000000000000000 ) ) ;
#13931 = CARTESIAN_POINT ( 'NONE',  ( 235.3564303562499447, -34.94062499938547717, 98.40857419181659793 ) ) ;
#13932 = CARTESIAN_POINT ( 'NONE',  ( -79.39999999999999147, -34.67268749875867684, 99.99999999999998579 ) ) ;
#13933 = ORIENTED_EDGE ( 'NONE', *, *, #15583, .T. ) ;
#13934 = EDGE_CURVE ( 'NONE', #14052, #3491, #18348, .T. ) ;
#13935 = CARTESIAN_POINT ( 'NONE',  ( -85.15643035624999868, -35.16562499938547859, 101.5914258081833879 ) ) ;
#13936 = DIRECTION ( 'NONE',  ( 0.000000000000000000, 0.000000000000000000, -1.000000000000000000 ) ) ;
#13937 = CYLINDRICAL_SURFACE ( 'NONE', #2377, 6.000000000000005329 ) ;
#13938 = DIRECTION ( 'NONE',  ( -1.000000000000000000, 0.000000000000000000, 0.000000000000000000 ) ) ;
#13939 = CYLINDRICAL_SURFACE ( 'NONE', #14885, 3.000000000000002665 ) ;
#13940 = AXIS2_PLACEMENT_3D ( 'NONE', #8518, #9800, #4036 ) ;
#13941 = CARTESIAN_POINT ( 'NONE',  ( 85.15643035624999868, -30.29062499938548925, -98.40857419181659793 ) ) ;
#13942 = CARTESIAN_POINT ( 'NONE',  ( 4.104070371397480876, 2.023683613428366002, 3.505122836902507810 ) ) ;
#13943 = ORIENTED_EDGE ( 'NONE', *, *, #9035, .T. ) ;
#13944 = CARTESIAN_POINT ( 'NONE',  ( 82.39999999999999147, -30.50624999877097210, 103.4641016151377499 ) ) ;
#13945 = PRODUCT_CONTEXT ( 'NONE', #18425, 'mechanical' ) ;
#13946 = CARTESIAN_POINT ( 'NONE',  ( 235.3564303562499447, -33.21562499938548285, 101.5914258081833879 ) ) ;
#13947 = CARTESIAN_POINT ( 'NONE',  ( 235.3564303562499447, -30.51562499938548001, -48.40857419181671162 ) ) ;
#13948 = AXIS2_PLACEMENT_3D ( 'NONE', #965, #18743, #1147 ) ;
#13949 = CARTESIAN_POINT ( 'NONE',  ( -83.77821517812500929, -32.76562499938548711, 102.3871387122750889 ) ) ;
#13950 = CARTESIAN_POINT ( 'NONE',  ( -79.64356964374998427, -34.82812499938548711, 98.40857419181659793 ) ) ;
#13951 = VERTEX_POINT ( 'NONE', #16878 ) ;
#13952 = ORIENTED_EDGE ( 'NONE', *, *, #18321, .F. ) ;
#13953 = CARTESIAN_POINT ( 'NONE',  ( -82.39999999999999147, -31.82812499938548356, -96.81714838363319586 ) ) ;
#13954 = DIRECTION ( 'NONE',  ( -0.000000000000000000, -1.000000000000000000, -0.000000000000000000 ) ) ;
#13955 = DIRECTION ( 'NONE',  ( -0.000000000000000000, 0.000000000000000000, 1.000000000000000000 ) ) ;
#13956 = ORIENTED_EDGE ( 'NONE', *, *, #8958, .T. ) ;
#13957 = DIRECTION ( 'NONE',  ( 0.000000000000000000, 0.000000000000000000, 1.000000000000000000 ) ) ;
#13958 = CARTESIAN_POINT ( 'NONE',  ( -85.40000000000000568, -34.93124999877096570, -101.7320508075688679 ) ) ;
#13959 = CARTESIAN_POINT ( 'NONE',  ( -81.59615242270662350, -31.93259618943233846, 97.00000000000000000 ) ) ;
#13960 = CARTESIAN_POINT ( 'NONE',  ( -79.39999999999999147, -31.03124999877097068, 98.26794919243110371 ) ) ;
#13961 = CARTESIAN_POINT ( 'NONE',  ( -79.39999999999999147, -35.08124999877097139, 98.26794919243110371 ) ) ;
#13962 = AXIS2_PLACEMENT_3D ( 'NONE', #18354, #769, #7796 ) ;
#13963 = CARTESIAN_POINT ( 'NONE',  ( -79.39999999999999147, -30.58124999877097139, 98.26794919243110371 ) ) ;
#13964 =( BOUNDED_SURFACE ( )  B_SPLINE_SURFACE ( 1, 2, ( 
 ( #14706, #75, #1432, #7196, #1537, #8850, #16479, #7486, #170, #10609, #8942, #15008, #13441, #4365, #13245, #17758, #19217, #2802, #17655, #3083, #11975, #5834, #18049, #14806, #13145, #6121, #7387, #1626, #10228, #14909, #16195, #13348, #17943, #13532, #11786, #10325, #16284, #7581, #19119, #11879, #4554, #2894, #8754, #18630, #5932, #4659, #16576, #17847, #1343, #3176, #10511, #7290, #4459, #10414, #16377, #2986, #9136, #5738, #11687, #3566, #15192, #11083, #1810, #10701, #16758, #3374, #3466, #18423, #654, #10796, #12364, #2103, #9326, #5044, #7773, #6602, #12270, #16667, #461, #10893, #4758, #9424, #13916, #9525, #1905, #3665, #3272, #6512, #15491, #13726, #18234, #6409, #15392, #367, #554, #14018, #12170, #4851, #15290, #13626, #5138, #8063, #9629, #6316, #7867, #13818, #12550, #1716, #17053, #7670, #12457, #18332, #4951, #18521, #269, #16861, #2003, #7962, #6223, #10985, #16954, #18138, #9228, #8806, #7342, #8514, #13295, #17607, #10282, #5887, #11739, #5785, #2753, #14763, #15951 ),
 ( #14465, #14663, #17706, #16143, #16244, #1298, #19271, #14562, #1097, #4220, #10178, #8710, #7157, #7056, #2199, #2552, #13015, #7245, #4321, #11647, #19173, #2646, #747, #2851, #11836, #1393, #17804, #5238, #18985, #4414, #16044, #15591, #5608, #8612, #11552, #8161, #6702, #11187, #14110, #18620, #19076, #13201, #12646, #9722, #17150, #3757, #17515, #4126, #13107, #10088, #1199, #5694, #6275, #17902, #3229, #4612, #18285, #4711, #12027, #328, #10656, #3324, #13779, #12130, #18190, #16623, #7534, #16431, #1584, #3040, #9001, #10371, #10464, #14961, #9188, #1768, #13583, #6081, #15150, #13398, #1865, #16335, #4509, #10567, #224, #13490, #7728, #12220, #13684, #4811, #131, #7440, #10752, #18100, #16716, #9284, #15252, #2944, #7824, #419, #6367, #18000, #16531, #12319, #8897, #14860, #6178, #5980, #1487, #30, #11930, #3132, #9091, #15054, #1678, #7629, #3615, #9577, #6559, #3520, #13972, #1959, #14257, #8115, #7918, #610, #15641, #15441, #895, #3805, #15343, #17200, #6658, #9478, #15544 ) ),
 .UNSPECIFIED., .F., .F., .F. ) 
 B_SPLINE_SURFACE_WITH_KNOTS ( ( 2, 2 ),
 ( 3, 2, 2, 2, 2, 2, 2, 2, 2, 2, 2, 2, 2, 2, 2, 2, 2, 2, 2, 2, 2, 2, 2, 2, 2, 2, 2, 2, 2, 2, 2, 2, 2, 2, 2, 2, 2, 2, 2, 2, 2, 2, 2, 2, 2, 2, 2, 2, 2, 2, 2, 2, 2, 2, 2, 2, 2, 2, 2, 2, 2, 2, 2, 2, 2, 2, 2, 3 ),
 ( 0.000000000000000000, 1.000000000000000000 ),
 ( 0.000000000000000000, 0.01388888888888888812, 0.02777777777777777624, 0.04166666666666666435, 0.05555555555555555247, 0.06944444444444444753, 0.08333333333333332871, 0.09722222222222222376, 0.1111111111111111049, 0.1250000000000000000, 0.1388888888888888951, 0.1527777777777777901, 0.1666666666666666574, 0.1805555555555555525, 0.1944444444444444475, 0.2083333333333333426, 0.2222222222222222099, 0.2361111111111111049, 0.2500000000000000000, 0.2638888888888888951, 0.2777777777777777901, 0.2916666666666666852, 0.3055555555555555802, 0.3194444444444444198, 0.3333333333333333148, 0.3472222222222222099, 0.3611111111111111049, 0.3750000000000000000, 0.3888888888888888951, 0.4027777777777777901, 0.4166666666666666852, 0.4305555555555555802, 0.4444444444444444198, 0.4583333333333333148, 0.4722222222222222099, 0.4861111111111111049, 0.5000000000000000000, 0.5138888888888888395, 0.5277777777777777901, 0.5416666666666666297, 0.5555555555555555802, 0.5694444444444444198, 0.5833333333333333703, 0.5972222222222222099, 0.6111111111111111605, 0.6250000000000000000, 0.6388888888888888395, 0.6527777777777777901, 0.6666666666666666297, 0.6805555555555555802, 0.6944444444444444198, 0.7083333333333333703, 0.7222222222222222099, 0.7361111111111111605, 0.7500000000000000000, 0.7638888888888888395, 0.7777777777777777901, 0.7916666666666666297, 0.8055555555555555802, 0.8194444444444444198, 0.8333333333333333703, 0.8472222222222222099, 0.8611111111111111605, 0.8750000000000000000, 0.8888888888888888395, 0.9027777777777777901, 0.9166666666666666297, 0.9258785565094813652 ),
 .UNSPECIFIED. ) 
 GEOMETRIC_REPRESENTATION_ITEM ( )  RATIONAL_B_SPLINE_SURFACE ( (
 ( 1.000000000000000000, 0.8660254037844387076, 1.000000000000000000, 0.8660254037844387076, 1.000000000000000000, 0.8660254037844387076, 1.000000000000000000, 0.8660254037844387076, 1.000000000000000000, 0.8660254037844387076, 1.000000000000000000, 0.8660254037844387076, 1.000000000000000000, 0.8660254037844387076, 1.000000000000000000, 0.8660254037844387076, 1.000000000000000000, 0.8660254037844387076, 1.000000000000000000, 0.8660254037844387076, 1.000000000000000000, 0.8660254037844387076, 1.000000000000000000, 0.8660254037844387076, 1.000000000000000000, 0.8660254037844387076, 1.000000000000000000, 0.8660254037844387076, 1.000000000000000000, 0.8660254037844387076, 1.000000000000000000, 0.8660254037844387076, 1.000000000000000000, 0.8660254037844387076, 1.000000000000000000, 0.8660254037844387076, 1.000000000000000000, 0.8660254037844387076, 1.000000000000000000, 0.8660254037844387076, 1.000000000000000000, 0.8660254037844387076, 1.000000000000000000, 0.8660254037844387076, 1.000000000000000000, 0.8660254037844387076, 1.000000000000000000, 0.8660254037844387076, 1.000000000000000000, 0.8660254037844387076, 1.000000000000000000, 0.8660254037844387076, 1.000000000000000000, 0.8660254037844387076, 1.000000000000000000, 0.8660254037844387076, 1.000000000000000000, 0.8660254037844387076, 1.000000000000000000, 0.8660254037844387076, 1.000000000000000000, 0.8660254037844387076, 1.000000000000000000, 0.8660254037844387076, 1.000000000000000000, 0.8660254037844387076, 1.000000000000000000, 0.8660254037844387076, 1.000000000000000000, 0.8660254037844387076, 1.000000000000000000, 0.8660254037844387076, 1.000000000000000000, 0.8660254037844387076, 1.000000000000000000, 0.8660254037844387076, 1.000000000000000000, 0.8660254037844387076, 1.000000000000000000, 0.8660254037844387076, 1.000000000000000000, 0.8660254037844387076, 1.000000000000000000, 0.8660254037844387076, 1.000000000000000000, 0.8660254037844387076, 1.000000000000000000, 0.8660254037844387076, 1.000000000000000000, 0.8660254037844387076, 1.000000000000000000, 0.8660254037844387076, 1.000000000000000000, 0.8660254037844387076, 1.000000000000000000, 0.8660254037844387076, 1.000000000000000000, 0.8660254037844387076, 1.000000000000000000, 0.8660254037844387076, 1.000000000000000000, 0.8660254037844387076, 1.000000000000000000, 0.8660254037844387076, 1.000000000000000000, 0.8660254037844387076, 1.000000000000000000, 0.8660254037844387076, 1.000000000000000000, 0.8660254037844387076, 1.000000000000000000, 0.8660254037844387076, 1.000000000000000000, 0.8660254037844387076, 1.000000000000000000, 0.8660254037844387076, 1.000000000000000000, 0.8660254037844387076, 1.000000000000000000, 0.8660254037844387076, 1.000000000000000000, 0.8660254037844387076, 1.000000000000000000, 0.8660254037844387076, 1.000000000000000000, 0.8660254037844387076, 1.000000000000000000, 0.8660254037844387076, 1.000000000000000000, 0.8660254037844387076, 1.000000000000000000, 0.8660254037844387076, 1.000000000000000000, 0.9111405360107203144, 0.9401542295229963209),
 ( 1.000000000000000000, 0.8660254037844387076, 1.000000000000000000, 0.8660254037844387076, 1.000000000000000000, 0.8660254037844387076, 1.000000000000000000, 0.8660254037844387076, 1.000000000000000000, 0.8660254037844387076, 1.000000000000000000, 0.8660254037844387076, 1.000000000000000000, 0.8660254037844387076, 1.000000000000000000, 0.8660254037844387076, 1.000000000000000000, 0.8660254037844387076, 1.000000000000000000, 0.8660254037844387076, 1.000000000000000000, 0.8660254037844387076, 1.000000000000000000, 0.8660254037844387076, 1.000000000000000000, 0.8660254037844387076, 1.000000000000000000, 0.8660254037844387076, 1.000000000000000000, 0.8660254037844387076, 1.000000000000000000, 0.8660254037844387076, 1.000000000000000000, 0.8660254037844387076, 1.000000000000000000, 0.8660254037844387076, 1.000000000000000000, 0.8660254037844387076, 1.000000000000000000, 0.8660254037844387076, 1.000000000000000000, 0.8660254037844387076, 1.000000000000000000, 0.8660254037844387076, 1.000000000000000000, 0.8660254037844387076, 1.000000000000000000, 0.8660254037844387076, 1.000000000000000000, 0.8660254037844387076, 1.000000000000000000, 0.8660254037844387076, 1.000000000000000000, 0.8660254037844387076, 1.000000000000000000, 0.8660254037844387076, 1.000000000000000000, 0.8660254037844387076, 1.000000000000000000, 0.8660254037844387076, 1.000000000000000000, 0.8660254037844387076, 1.000000000000000000, 0.8660254037844387076, 1.000000000000000000, 0.8660254037844387076, 1.000000000000000000, 0.8660254037844387076, 1.000000000000000000, 0.8660254037844387076, 1.000000000000000000, 0.8660254037844387076, 1.000000000000000000, 0.8660254037844387076, 1.000000000000000000, 0.8660254037844387076, 1.000000000000000000, 0.8660254037844387076, 1.000000000000000000, 0.8660254037844387076, 1.000000000000000000, 0.8660254037844387076, 1.000000000000000000, 0.8660254037844387076, 1.000000000000000000, 0.8660254037844387076, 1.000000000000000000, 0.8660254037844387076, 1.000000000000000000, 0.8660254037844387076, 1.000000000000000000, 0.8660254037844387076, 1.000000000000000000, 0.8660254037844387076, 1.000000000000000000, 0.8660254037844387076, 1.000000000000000000, 0.8660254037844387076, 1.000000000000000000, 0.8660254037844387076, 1.000000000000000000, 0.8660254037844387076, 1.000000000000000000, 0.8660254037844387076, 1.000000000000000000, 0.8660254037844387076, 1.000000000000000000, 0.8660254037844387076, 1.000000000000000000, 0.8660254037844387076, 1.000000000000000000, 0.8660254037844387076, 1.000000000000000000, 0.8660254037844387076, 1.000000000000000000, 0.8660254037844387076, 1.000000000000000000, 0.8660254037844387076, 1.000000000000000000, 0.8660254037844387076, 1.000000000000000000, 0.8660254037844387076, 1.000000000000000000, 0.8660254037844387076, 1.000000000000000000, 0.8660254037844387076, 1.000000000000000000, 0.8660254037844387076, 1.000000000000000000, 0.8660254037844387076, 1.000000000000000000, 0.8660254037844387076, 1.000000000000000000, 0.9111405360107203144, 0.9401542295229963209) ) ) 
 REPRESENTATION_ITEM ( '' )  SURFACE ( )  );
#13965 = STYLED_ITEM ( 'NONE', ( #2158 ), #16702 ) ;
#13966 = CARTESIAN_POINT ( 'NONE',  ( 229.5999999999999375, -33.99374999877096570, -50.00000000000011369 ) ) ;
#13967 = DIRECTION ( 'NONE',  ( 1.000000000000000000, 5.337610695313256118E-15, 0.000000000000000000 ) ) ;
#13968 = CARTESIAN_POINT ( 'NONE',  ( 229.8435696437499871, -33.70312499938548001, 101.5914258081833879 ) ) ;
#13969 = ORIENTED_EDGE ( 'NONE', *, *, #11532, .T. ) ;
#13970 = AXIS2_PLACEMENT_3D ( 'NONE', #11510, #15813, #11599 ) ;
#13971 =( LENGTH_UNIT ( ) NAMED_UNIT ( * ) SI_UNIT ( .MILLI., .METRE. ) );
#13972 = CARTESIAN_POINT ( 'NONE',  ( -85.15643035625001289, -34.64062499938548711, -99.99999999999998579 ) ) ;
#13973 = PLANE ( 'NONE',  #558 ) ;
#13974 = ORIENTED_EDGE ( 'NONE', *, *, #162, .T. ) ;
#13975 = FACE_OUTER_BOUND ( 'NONE', #6410, .T. ) ;
#13976 = CARTESIAN_POINT ( 'NONE',  ( 2.000000000000005329, -3.464101615137751722, 0.000000000000000000 ) ) ;
#13977 = EDGE_LOOP ( 'NONE', ( #181, #8090, #14135, #4161 ) ) ;
#13978 = CARTESIAN_POINT ( 'NONE',  ( 229.8435696437499303, -34.64062499938548001, -50.00000000000011369 ) ) ;
#13979 = AXIS2_PLACEMENT_3D ( 'NONE', #1454, #14934, #7407 ) ;
#13980 = AXIS2_PLACEMENT_3D ( 'NONE', #1005, #4027, #5689 ) ;
#13981 = ORIENTED_EDGE ( 'NONE', *, *, #17977, .F. ) ;
#13982 = ORIENTED_EDGE ( 'NONE', *, *, #14141, .F. ) ;
#13983 = CARTESIAN_POINT ( 'NONE',  ( 234.0999999999999375, -33.29999999999999716, -52.59807621135342970 ) ) ;
#13984 = CARTESIAN_POINT ( 'NONE',  ( 80.90000000000000568, -31.50000000000000000, -97.40192378864668399 ) ) ;
#13985 = DIRECTION ( 'NONE',  ( 0.000000000000000000, 0.000000000000000000, -1.000000000000000000 ) ) ;
#13986 = CARTESIAN_POINT ( 'NONE',  ( -85.40000000000000568, -35.34374999877096712, 99.99999999999998579 ) ) ;
#13987 = CARTESIAN_POINT ( 'NONE',  ( -80.90000000000000568, -34.79606250001229739, 102.5980762113533018 ) ) ;
#13988 = DIRECTION ( 'NONE',  ( 0.000000000000000000, 6.982962677686266711E-15, -1.000000000000000000 ) ) ;
#13989 = CARTESIAN_POINT ( 'NONE',  ( 82.39999999999999147, -33.06562499938548427, -96.81714838363319586 ) ) ;
#13990 = CARTESIAN_POINT ( 'NONE',  ( -80.90000000000000568, -33.45000000000000284, 102.5980762113533018 ) ) ;
#13991 = CARTESIAN_POINT ( 'NONE',  ( -82.39999999999999147, -33.62812499938549138, 103.1828516163667899 ) ) ;
#13992 = CARTESIAN_POINT ( 'NONE',  ( 85.15643035624999868, -33.70312499938548711, -101.5914258081833879 ) ) ;
#13993 = VERTEX_POINT ( 'NONE', #3482 ) ;
#13994 = CARTESIAN_POINT ( 'NONE',  ( -85.39999999999999147, -34.97364041986484295, 98.90809577818232867 ) ) ;
#13995 = ADVANCED_FACE ( 'NONE', ( #15408 ), #9442, .F. ) ;
#13996 = B_SPLINE_CURVE_WITH_KNOTS ( 'NONE', 3,
 ( #13882, #11249, #3629, #9591, #12519, #3537 ),
 .UNSPECIFIED., .F., .F.,
 ( 4, 2, 4 ),
 ( 0.000000000000000000, 0.002086519881787262786, 0.004173039763574524705 ),
 .UNSPECIFIED. ) ;
#13997 = EDGE_CURVE ( 'NONE', #5564, #15718, #4945, .T. ) ;
#13998 = CYLINDRICAL_SURFACE ( 'NONE', #2408, 3.000000000000002665 ) ;
#13999 = CARTESIAN_POINT ( 'NONE',  ( 233.9782151781249411, -33.55312499938548143, 97.61286128772489690 ) ) ;
#14000 = CARTESIAN_POINT ( 'NONE',  ( -85.15643035624999868, -31.64062499938548356, 98.40857419181659793 ) ) ;
#14001 = CARTESIAN_POINT ( 'NONE',  ( 232.5999999999999375, -32.61562499938548143, -53.18285161636690361 ) ) ;
#14002 = CARTESIAN_POINT ( 'NONE',  ( -79.39999999999999147, -32.02500000000000568, 99.99999999999998579 ) ) ;
#14003 = ORIENTED_EDGE ( 'NONE', *, *, #7428, .F. ) ;
#14004 = CARTESIAN_POINT ( 'NONE',  ( 4.180231680468789790, -2.085385483809537810, 3.570466434508605680 ) ) ;
#14005 = CARTESIAN_POINT ( 'NONE',  ( 82.49978216248237572, -34.99999999999998579, 97.23961338447999481 ) ) ;
#14006 = CARTESIAN_POINT ( 'NONE',  ( 83.77821517812500929, -33.36562499938548854, 102.3871387122750889 ) ) ;
#14007 = EDGE_CURVE ( 'NONE', #11485, #13696, #2132, .T. ) ;
#14008 = EDGE_CURVE ( 'NONE', #18284, #15758, #635, .T. ) ;
#14009 = CARTESIAN_POINT ( 'NONE',  ( 85.11512745526610502, -31.99999999999997868, -100.5952676699196218 ) ) ;
#14010 =( BOUNDED_CURVE ( )  B_SPLINE_CURVE ( 2, ( #17492, #4101, #10063, #16021, #2623, #16791, #9354, #6149, #392, #7893, #7701, #15032, #1839, #6344, #9258, #3402, #13658, #9067, #7798, #15316, #3109, #485, #6437, #1742, #13753, #3015, #7510, #18074, #1932, #13843, #17877, #15225, #12295, #4786, #1654, #4583, #10633, #16599, #4486, #18261, #3204, #10543, #4683, #12194, #4878, #10820, #18164, #10440, #9163, #16506, #8972, #16405, #6249, #17973, #7606, #299, #14938, #1563, #13467, #15127, #105, #10728, #6055, #16691, #199, #3300, #12002, #13557, #12100, #11012, #7988, #15516, #2221, #6832, #6536, #15809, #16888, #6726, #8187, #3492, #3691, #18357, #8377 ),
 .UNSPECIFIED., .F., .F. ) 
 B_SPLINE_CURVE_WITH_KNOTS ( ( 3, 2, 2, 2, 2, 2, 2, 2, 2, 2, 2, 2, 2, 2, 2, 2, 2, 2, 2, 2, 2, 2, 2, 2, 2, 2, 2, 2, 2, 2, 2, 2, 2, 2, 2, 2, 2, 2, 2, 2, 2, 3 ),
 ( 0.3495698921800969861, 0.3600184345287978371, 0.3750192026341644391, 0.3900199707395310411, 0.4050207388448976431, 0.4200215069502642451, 0.4350222750556308471, 0.4500230431609974491, 0.4650238112663640511, 0.4800245793717305975, 0.4950253474770971440, 0.5100261155824636905, 0.5250268836878303480, 0.5400276517931970055, 0.5550284198985635520, 0.5700291880039300985, 0.5850299561092966449, 0.6000307242146634135, 0.6150314923200298489, 0.6300322604253965064, 0.6450330285307630529, 0.6600337966361297104, 0.6750345647414962569, 0.6900353328468626923, 0.7050361009522294609, 0.7200368690575960073, 0.7350376371629626648, 0.7500384052683291003, 0.7650391733736958688, 0.7800399414790624153, 0.7950407095844289618, 0.8100414776897955083, 0.8250422457951620547, 0.8400430139005288233, 0.8550437820058953697, 0.8700445501112619162, 0.8850453182166284627, 0.9000460863219950092, 0.9150468544273615557, 0.9300476225327283242, 0.9450483906380948707, 0.9496006163947610101 ),
 .UNSPECIFIED. ) 
 CURVE ( )  GEOMETRIC_REPRESENTATION_ITEM ( )  RATIONAL_B_SPLINE_CURVE ( ( 0.9433623850486680951, 0.9066821623815655151, 1.000000000000000000, 0.8660254037844387076, 1.000000000000000000, 0.8660254037844387076, 1.000000000000000000, 0.8660254037844387076, 1.000000000000000000, 0.8660254037844387076, 1.000000000000000000, 0.8660254037844387076, 1.000000000000000000, 0.8660254037844387076, 1.000000000000000000, 0.8660254037844387076, 1.000000000000000000, 0.8660254037844387076, 1.000000000000000000, 0.8660254037844387076, 1.000000000000000000, 0.8660254037844387076, 1.000000000000000000, 0.8660254037844387076, 1.000000000000000000, 0.8660254037844387076, 1.000000000000000000, 0.8660254037844387076, 1.000000000000000000, 0.8660254037844387076, 1.000000000000000000, 0.8660254037844387076, 1.000000000000000000, 0.8660254037844387076, 1.000000000000000000, 0.8660254037844387076, 1.000000000000000000, 0.8660254037844387076, 1.000000000000000000, 0.8660254037844387076, 1.000000000000000000, 0.8660254037844387076, 1.000000000000000000, 0.8660254037844387076, 1.000000000000000000, 0.8660254037844387076, 1.000000000000000000, 0.8660254037844387076, 1.000000000000000000, 0.8660254037844387076, 1.000000000000000000, 0.8660254037844387076, 1.000000000000000000, 0.8660254037844387076, 1.000000000000000000, 0.8660254037844387076, 1.000000000000000000, 0.8660254037844387076, 1.000000000000000000, 0.8660254037844387076, 1.000000000000000000, 0.8660254037844387076, 1.000000000000000000, 0.8660254037844387076, 1.000000000000000000, 0.8660254037844387076, 1.000000000000000000, 0.8660254037844387076, 1.000000000000000000, 0.8660254037844387076, 1.000000000000000000, 0.8660254037844387076, 1.000000000000000000, 0.8660254037844387076, 1.000000000000000000, 0.8660254037844387076, 1.000000000000000000, 0.8660254037844387076, 1.000000000000000000, 0.8660254037844387076, 1.000000000000000000, 0.9593432414028693067, 0.9433623850486648754 ) ) 
 REPRESENTATION_ITEM ( '' )  );
#14011 = CARTESIAN_POINT ( 'NONE',  ( -81.02178482187500208, -31.75312499938548427, 97.61286128772489690 ) ) ;
#14012 = CARTESIAN_POINT ( 'NONE',  ( -79.64356964374998427, -32.31562499938548427, -98.40857419181659793 ) ) ;
#14013 = CARTESIAN_POINT ( 'NONE',  ( 85.15643035624999868, -31.90312499938548285, 98.40857419181659793 ) ) ;
#14014 = B_SPLINE_CURVE_WITH_KNOTS ( 'NONE', 3,
 ( #8739, #14693, #7277, #13231, #5821, #17745, #11769, #3455, #9412, #10880, #10783, #18034, #18317, #9124, #13521, #7565, #15087, #6496 ),
 .UNSPECIFIED., .F., .F.,
 ( 4, 2, 2, 2, 2, 2, 2, 2, 4 ),
 ( 0.000000000000000000, 0.0007089252359835931331, 0.001417850471967186266, 0.002126775707950779616, 0.002835700943934372532, 0.003544626179917965449, 0.004253551415901559232, 0.004962476651885152149, 0.005671401887868745065 ),
 .UNSPECIFIED. ) ;
#14015 = CARTESIAN_POINT ( 'NONE',  ( 82.39999999999999147, -32.16562499938549280, -96.81714838363319586 ) ) ;
#14016 = CARTESIAN_POINT ( 'NONE',  ( 233.9782151781249411, -31.19062499938547717, -52.38713871227520968 ) ) ;
#14017 = CARTESIAN_POINT ( 'NONE',  ( -85.15643035625001289, -32.99062499938548854, 98.40857419181659793 ) ) ;
#14018 = CARTESIAN_POINT ( 'NONE',  ( -85.15643035624999868, -33.81562499938549138, -98.40857419181659793 ) ) ;
#14019 = EDGE_CURVE ( 'NONE', #1510, #18598, #6913, .T. ) ;
#14020 = ORIENTED_EDGE ( 'NONE', *, *, #8877, .F. ) ;
#14021 = CARTESIAN_POINT ( 'NONE',  ( 82.39999999999999147, -32.61562499938548854, 103.1828516163667899 ) ) ;
#14022 = CARTESIAN_POINT ( 'NONE',  ( 233.4038475772933339, -34.18259618943231715, 97.00000000000000000 ) ) ;
#14023 = CARTESIAN_POINT ( 'NONE',  ( -81.02178482187500208, -30.44062499938548783, 102.3871387122750889 ) ) ;
#14024 = CARTESIAN_POINT ( 'NONE',  ( -81.02178482187500208, -33.55312499938548854, 97.61286128772489690 ) ) ;
#14025 = DIRECTION ( 'NONE',  ( -0.000000000000000000, -1.000000000000000000, -0.000000000000000000 ) ) ;
#14026 = ORIENTED_EDGE ( 'NONE', *, *, #13489, .F. ) ;
#14027 = CARTESIAN_POINT ( 'NONE',  ( -85.40000000000000568, -34.05000000000000426, -99.99999999999998579 ) ) ;
#14028 = PRODUCT_DEFINITION_SHAPE ( 'NONE', 'NONE',  #19331 ) ;
#14029 = CARTESIAN_POINT ( 'NONE',  ( 229.5999999999999375, -34.48124999877096286, -51.73205080756898866 ) ) ;
#14030 = DIRECTION ( 'NONE',  ( -0.000000000000000000, -1.000000000000000000, -0.000000000000000000 ) ) ;
#14031 = PLANE ( 'NONE',  #14512 ) ;
#14032 = CARTESIAN_POINT ( 'NONE',  ( 232.5999999999999375, -30.25312499938548072, 96.81714838363319586 ) ) ;
#14033 = CARTESIAN_POINT ( 'NONE',  ( -80.90000000000000568, -33.39768749875867826, 102.5980762113533018 ) ) ;
#14034 = VERTEX_POINT ( 'NONE', #8647 ) ;
#14035 = PLANE ( 'NONE',  #8663 ) ;
#14036 = LINE ( 'NONE', #7980, #11006 ) ;
#14037 = CARTESIAN_POINT ( 'NONE',  ( -85.40000000000000568, -33.14999999999999858, 99.99999999999998579 ) ) ;
#14038 = CARTESIAN_POINT ( 'NONE',  ( 83.20384757729337366, -34.35134618820330843, -103.0000000000000000 ) ) ;
#14039 = CARTESIAN_POINT ( 'NONE',  ( 83.90000000000000568, -32.77499999999999858, -97.40192378864668399 ) ) ;
#14040 = CARTESIAN_POINT ( 'NONE',  ( 82.39999999999999147, -31.04062499938548569, -103.1828516163667899 ) ) ;
#14041 = CARTESIAN_POINT ( 'NONE',  ( 234.0999999999999375, -34.79999999999999716, 102.5980762113533018 ) ) ;
#14042 =( BOUNDED_CURVE ( )  B_SPLINE_CURVE ( 2, ( #16029, #8788, #10163, #4399, #17885, #2630, #17591 ),
 .UNSPECIFIED., .F., .F. ) 
 B_SPLINE_CURVE_WITH_KNOTS ( ( 3, 2, 2, 3 ),
 ( 0.3702305174533208065, 0.3750000000000000000, 0.3888888888888888951, 0.3958333333333334259 ),
 .UNSPECIFIED. ) 
 CURVE ( )  GEOMETRIC_REPRESENTATION_ITEM ( )  RATIONAL_B_SPLINE_CURVE ( ( 0.9395835397642970932, 0.9539927561189072147, 1.000000000000000000, 0.8660254037844387076, 1.000000000000000000, 0.9330127018922185211, 0.9330127018922192983 ) ) 
 REPRESENTATION_ITEM ( '' )  );
#14043 = ORIENTED_EDGE ( 'NONE', *, *, #2420, .F. ) ;
#14044 = CARTESIAN_POINT ( 'NONE',  ( 82.39999999999999147, -31.63124999877097210, 96.53589838486223584 ) ) ;
#14045 = PRODUCT_CONTEXT ( 'NONE', #6080, 'mechanical' ) ;
#14046 = CARTESIAN_POINT ( 'NONE',  ( 235.3564303562499447, -32.72812499938547859, 99.99999999999998579 ) ) ;
#14047 = CARTESIAN_POINT ( 'NONE',  ( 229.8435696437499871, -30.29062499938548214, -51.59142580818350865 ) ) ;
#14048 = CARTESIAN_POINT ( 'NONE',  ( -82.39999999999999147, -34.52812499938548996, 103.1828516163667899 ) ) ;
#14049 = CARTESIAN_POINT ( 'NONE',  ( -79.64356964374998427, -34.90312499938548285, 101.5914258081833879 ) ) ;
#14050 = ORIENTED_EDGE ( 'NONE', *, *, #1497, .T. ) ;
#14052 = VERTEX_POINT ( 'NONE', #10126 ) ;
#14051 = EDGE_CURVE ( 'NONE', #6590, #9205, #7050, .T. ) ;
#14053 = CARTESIAN_POINT ( 'NONE',  ( -85.15643035625001289, -31.04062499938548569, -99.99999999999998579 ) ) ;
#14054 = CARTESIAN_POINT ( 'NONE',  ( -85.40000000000000568, -32.25000000000000000, -99.99999999999998579 ) ) ;
#14055 = ORIENTED_EDGE ( 'NONE', *, *, #3784, .T. ) ;
#14056 = CARTESIAN_POINT ( 'NONE',  ( 81.02178482187500208, -32.80312499938548854, 97.61286128772489690 ) ) ;
#14057 = CARTESIAN_POINT ( 'NONE',  ( -79.39999999999999147, -34.21874999877096712, -99.99999999999998579 ) ) ;
#14058 = CARTESIAN_POINT ( 'NONE',  ( 80.90000000000000568, -32.10000000000000142, 97.40192378864668399 ) ) ;
#14059 = CARTESIAN_POINT ( 'NONE',  ( -81.59615242270662350, -34.18259618943233136, 96.99999999999998579 ) ) ;
#14060 = CARTESIAN_POINT ( 'NONE',  ( -80.90000000000000568, -32.49374999877097281, 102.5980762113533018 ) ) ;
#14061 = CARTESIAN_POINT ( 'NONE',  ( -85.40000000000000568, -33.54374999877096286, 99.99999999999998579 ) ) ;
#14062 = CARTESIAN_POINT ( 'NONE',  ( 82.40000000000000568, -30.00000000000000355, 99.99999999999998579 ) ) ;
#14063 = CARTESIAN_POINT ( 'NONE',  ( 233.4038475772933054, -32.51115380933862298, 102.9999999999999858 ) ) ;
#14064 = CARTESIAN_POINT ( 'NONE',  ( 94.79999999999995453, -5.200000000000000178, 150.0000000000000000 ) ) ;
#14065 = CARTESIAN_POINT ( 'NONE',  ( 229.8435696437499871, -32.87812499938547717, 98.40857419181659793 ) ) ;
#14066 = VERTEX_POINT ( 'NONE', #3968 ) ;
#14067 = CARTESIAN_POINT ( 'NONE',  ( 81.02178482187500208, -33.14062499938548711, -102.3871387122750889 ) ) ;
#14068 = SHAPE_REPRESENTATION_RELATIONSHIP ( 'NONE' , 'NONE' ,  #16991, #18578 ) ;
#14069 = CARTESIAN_POINT ( 'NONE',  ( 235.5999999999999375, -31.06874999877096144, 99.99999999999998579 ) ) ;
#14070 = CARTESIAN_POINT ( 'NONE',  ( -80.90000000000000568, -32.79374999877096997, -102.5980762113533018 ) ) ;
#14071 = ORIENTED_EDGE ( 'NONE', *, *, #704, .F. ) ;
#14072 = CARTESIAN_POINT ( 'NONE',  ( -82.40000000000001990, -33.26250000000000284, -103.0000000000000000 ) ) ;
#14073 = CARTESIAN_POINT ( 'NONE',  ( 82.85452780460281019, -34.99999999999999289, -102.7245357809972575 ) ) ;
#14074 = DIRECTION ( 'NONE',  ( -1.000000000000000000, 1.586032892321652482E-15, -0.000000000000000000 ) ) ;
#14075 = ORIENTED_EDGE ( 'NONE', *, *, #17376, .T. ) ;
#14076 = CARTESIAN_POINT ( 'NONE',  ( 4.151274195509476073, -2.039912954708822834, 3.533232880573632606 ) ) ;
#14077 = ORIENTED_EDGE ( 'NONE', *, *, #2183, .T. ) ;
#14078 = CARTESIAN_POINT ( 'NONE',  ( 79.39999999999999147, -30.26249999999999929, -101.7320508075688537 ) ) ;
#14079 = CARTESIAN_POINT ( 'NONE',  ( 0.000000000000000000, 0.000000000000000000, -4.694516984716113228 ) ) ;
#14080 =( BOUNDED_SURFACE ( )  B_SPLINE_SURFACE ( 1, 2, ( 
 ( #9377, #11237, #2343, #8216, #797, #508, #16911, #12800, #5096, #15737, #18474, #11040, #17005, #8304, #6460, #12414, #6854, #18383, #14069, #11134, #17103, #5004, #10943, #705, #10848, #12603, #18575, #3714, #4901, #9679, #6756, #2246, #18674, #16820, #3427, #13085, #1077, #8691, #19054, #11715, #2829, #1176, #7222, #5676, #15927, #5488, #9973, #11434, #17395, #7319, #18865, #4010, #17585, #10158, #2625, #14445, #11620, #2445, #10260, #5388, #12895, #12990, #8587, #2529, #4197, #1275, #16121, #13177, #8490, #15833, #7035, #8400, #18962, #5584, #7134, #2729, #17683, #11530, #10064, #19150, #17493, #14641, #4103, #4296, #16023, #14352, #14540, #5763, #988, #16223, #8783, #14737, #1372, #18766, #6944, #11334, #17299, #3905, #9871, #17975, #7608, #7415, #12102, #6251, #4392, #10442, #14940, #5864, #16693, #15129, #1841, #10, #8974, #16406, #4788, #13272, #3302, #19247, #18076, #1565, #5959, #1745, #11816, #4488, #11907, #3016, #9260, #10635, #12004, #10730, #10349, #12196, #15227, #17880, #17785 ),
 ( #7511, #13560, #16314, #2923, #8875, #13376, #13468, #3110, #107, #4684, #7703, #201, #13660, #6058, #14835, #16601, #15033, #3206, #9165, #18166, #1461, #301, #4585, #10545, #16507, #9069, #1656, #6151, #393, #11014, #3404, #9658, #4879, #2136, #3494, #11215, #15617, #16794, #14139, #6537, #12483, #9453, #6439, #16890, #10822, #17180, #16980, #9357, #15419, #18547, #18359, #3783, #6727, #18263, #774, #9552, #12581, #18647, #486, #12674, #12297, #15318, #5270, #1934, #3592, #8092, #14046, #7895, #13845, #12390, #13755, #4981, #18452, #10922, #9750, #2030, #3692, #7990, #681, #13946, #15714, #6632, #586, #17078, #5164, #7800, #6345, #15518, #2223, #11110, #5073, #8189, #12871, #14330, #8379, #10233, #2415, #6923, #1150, #13064, #5557, #17369, #15999, #5365, #13148, #8282, #15810, #15904, #11507, #968, #7108, #4176, #2603, #16096, #18842, #18747, #19029, #4079, #5651, #11596, #7199, #2318, #17564, #11690, #2701, #5465, #11409, #10136, #8564, #14231, #17468, #17278, #8660, #11312, #14517 ) ),
 .UNSPECIFIED., .F., .F., .F. ) 
 B_SPLINE_SURFACE_WITH_KNOTS ( ( 2, 2 ),
 ( 3, 2, 2, 2, 2, 2, 2, 2, 2, 2, 2, 2, 2, 2, 2, 2, 2, 2, 2, 2, 2, 2, 2, 2, 2, 2, 2, 2, 2, 2, 2, 2, 2, 2, 2, 2, 2, 2, 2, 2, 2, 2, 2, 2, 2, 2, 2, 2, 2, 2, 2, 2, 2, 2, 2, 2, 2, 2, 2, 2, 2, 2, 2, 2, 2, 2, 2, 3 ),
 ( 0.000000000000000000, 1.000000000000000000 ),
 ( 0.000000000000000000, 0.01388888888888888812, 0.02777777777777777624, 0.04166666666666666435, 0.05555555555555555247, 0.06944444444444444753, 0.08333333333333332871, 0.09722222222222222376, 0.1111111111111111049, 0.1250000000000000000, 0.1388888888888888951, 0.1527777777777777901, 0.1666666666666666574, 0.1805555555555555525, 0.1944444444444444475, 0.2083333333333333426, 0.2222222222222222099, 0.2361111111111111049, 0.2500000000000000000, 0.2638888888888888951, 0.2777777777777777901, 0.2916666666666666852, 0.3055555555555555802, 0.3194444444444444198, 0.3333333333333333148, 0.3472222222222222099, 0.3611111111111111049, 0.3750000000000000000, 0.3888888888888888951, 0.4027777777777777901, 0.4166666666666666852, 0.4305555555555555802, 0.4444444444444444198, 0.4583333333333333148, 0.4722222222222222099, 0.4861111111111111049, 0.5000000000000000000, 0.5138888888888888395, 0.5277777777777777901, 0.5416666666666666297, 0.5555555555555555802, 0.5694444444444444198, 0.5833333333333333703, 0.5972222222222222099, 0.6111111111111111605, 0.6250000000000000000, 0.6388888888888888395, 0.6527777777777777901, 0.6666666666666666297, 0.6805555555555555802, 0.6944444444444444198, 0.7083333333333333703, 0.7222222222222222099, 0.7361111111111111605, 0.7500000000000000000, 0.7638888888888888395, 0.7777777777777777901, 0.7916666666666666297, 0.8055555555555555802, 0.8194444444444444198, 0.8333333333333333703, 0.8472222222222222099, 0.8611111111111111605, 0.8750000000000000000, 0.8888888888888888395, 0.9027777777777777901, 0.9166666666666666297, 0.9258785144422092550 ),
 .UNSPECIFIED. ) 
 GEOMETRIC_REPRESENTATION_ITEM ( )  RATIONAL_B_SPLINE_SURFACE ( (
 ( 1.000000000000000000, 0.8660254037844387076, 1.000000000000000000, 0.8660254037844387076, 1.000000000000000000, 0.8660254037844387076, 1.000000000000000000, 0.8660254037844387076, 1.000000000000000000, 0.8660254037844387076, 1.000000000000000000, 0.8660254037844387076, 1.000000000000000000, 0.8660254037844387076, 1.000000000000000000, 0.8660254037844387076, 1.000000000000000000, 0.8660254037844387076, 1.000000000000000000, 0.8660254037844387076, 1.000000000000000000, 0.8660254037844387076, 1.000000000000000000, 0.8660254037844387076, 1.000000000000000000, 0.8660254037844387076, 1.000000000000000000, 0.8660254037844387076, 1.000000000000000000, 0.8660254037844387076, 1.000000000000000000, 0.8660254037844387076, 1.000000000000000000, 0.8660254037844387076, 1.000000000000000000, 0.8660254037844387076, 1.000000000000000000, 0.8660254037844387076, 1.000000000000000000, 0.8660254037844387076, 1.000000000000000000, 0.8660254037844387076, 1.000000000000000000, 0.8660254037844387076, 1.000000000000000000, 0.8660254037844387076, 1.000000000000000000, 0.8660254037844387076, 1.000000000000000000, 0.8660254037844387076, 1.000000000000000000, 0.8660254037844387076, 1.000000000000000000, 0.8660254037844387076, 1.000000000000000000, 0.8660254037844387076, 1.000000000000000000, 0.8660254037844387076, 1.000000000000000000, 0.8660254037844387076, 1.000000000000000000, 0.8660254037844387076, 1.000000000000000000, 0.8660254037844387076, 1.000000000000000000, 0.8660254037844387076, 1.000000000000000000, 0.8660254037844387076, 1.000000000000000000, 0.8660254037844387076, 1.000000000000000000, 0.8660254037844387076, 1.000000000000000000, 0.8660254037844387076, 1.000000000000000000, 0.8660254037844387076, 1.000000000000000000, 0.8660254037844387076, 1.000000000000000000, 0.8660254037844387076, 1.000000000000000000, 0.8660254037844387076, 1.000000000000000000, 0.8660254037844387076, 1.000000000000000000, 0.8660254037844387076, 1.000000000000000000, 0.8660254037844387076, 1.000000000000000000, 0.8660254037844387076, 1.000000000000000000, 0.8660254037844387076, 1.000000000000000000, 0.8660254037844387076, 1.000000000000000000, 0.8660254037844387076, 1.000000000000000000, 0.8660254037844387076, 1.000000000000000000, 0.8660254037844387076, 1.000000000000000000, 0.8660254037844387076, 1.000000000000000000, 0.8660254037844387076, 1.000000000000000000, 0.8660254037844387076, 1.000000000000000000, 0.8660254037844387076, 1.000000000000000000, 0.8660254037844387076, 1.000000000000000000, 0.8660254037844387076, 1.000000000000000000, 0.8660254037844387076, 1.000000000000000000, 0.8660254037844387076, 1.000000000000000000, 0.8660254037844387076, 1.000000000000000000, 0.8660254037844387076, 1.000000000000000000, 0.8660254037844387076, 1.000000000000000000, 0.8660254037844387076, 1.000000000000000000, 0.8660254037844387076, 1.000000000000000000, 0.8660254037844387076, 1.000000000000000000, 0.8660254037844387076, 1.000000000000000000, 0.8660254037844387076, 1.000000000000000000, 0.9111409417988175496, 0.9401539645359766606),
 ( 1.000000000000000000, 0.8660254037844387076, 1.000000000000000000, 0.8660254037844387076, 1.000000000000000000, 0.8660254037844387076, 1.000000000000000000, 0.8660254037844387076, 1.000000000000000000, 0.8660254037844387076, 1.000000000000000000, 0.8660254037844387076, 1.000000000000000000, 0.8660254037844387076, 1.000000000000000000, 0.8660254037844387076, 1.000000000000000000, 0.8660254037844387076, 1.000000000000000000, 0.8660254037844387076, 1.000000000000000000, 0.8660254037844387076, 1.000000000000000000, 0.8660254037844387076, 1.000000000000000000, 0.8660254037844387076, 1.000000000000000000, 0.8660254037844387076, 1.000000000000000000, 0.8660254037844387076, 1.000000000000000000, 0.8660254037844387076, 1.000000000000000000, 0.8660254037844387076, 1.000000000000000000, 0.8660254037844387076, 1.000000000000000000, 0.8660254037844387076, 1.000000000000000000, 0.8660254037844387076, 1.000000000000000000, 0.8660254037844387076, 1.000000000000000000, 0.8660254037844387076, 1.000000000000000000, 0.8660254037844387076, 1.000000000000000000, 0.8660254037844387076, 1.000000000000000000, 0.8660254037844387076, 1.000000000000000000, 0.8660254037844387076, 1.000000000000000000, 0.8660254037844387076, 1.000000000000000000, 0.8660254037844387076, 1.000000000000000000, 0.8660254037844387076, 1.000000000000000000, 0.8660254037844387076, 1.000000000000000000, 0.8660254037844387076, 1.000000000000000000, 0.8660254037844387076, 1.000000000000000000, 0.8660254037844387076, 1.000000000000000000, 0.8660254037844387076, 1.000000000000000000, 0.8660254037844387076, 1.000000000000000000, 0.8660254037844387076, 1.000000000000000000, 0.8660254037844387076, 1.000000000000000000, 0.8660254037844387076, 1.000000000000000000, 0.8660254037844387076, 1.000000000000000000, 0.8660254037844387076, 1.000000000000000000, 0.8660254037844387076, 1.000000000000000000, 0.8660254037844387076, 1.000000000000000000, 0.8660254037844387076, 1.000000000000000000, 0.8660254037844387076, 1.000000000000000000, 0.8660254037844387076, 1.000000000000000000, 0.8660254037844387076, 1.000000000000000000, 0.8660254037844387076, 1.000000000000000000, 0.8660254037844387076, 1.000000000000000000, 0.8660254037844387076, 1.000000000000000000, 0.8660254037844387076, 1.000000000000000000, 0.8660254037844387076, 1.000000000000000000, 0.8660254037844387076, 1.000000000000000000, 0.8660254037844387076, 1.000000000000000000, 0.8660254037844387076, 1.000000000000000000, 0.8660254037844387076, 1.000000000000000000, 0.8660254037844387076, 1.000000000000000000, 0.8660254037844387076, 1.000000000000000000, 0.8660254037844387076, 1.000000000000000000, 0.8660254037844387076, 1.000000000000000000, 0.8660254037844387076, 1.000000000000000000, 0.8660254037844387076, 1.000000000000000000, 0.8660254037844387076, 1.000000000000000000, 0.8660254037844387076, 1.000000000000000000, 0.8660254037844387076, 1.000000000000000000, 0.8660254037844387076, 1.000000000000000000, 0.8660254037844387076, 1.000000000000000000, 0.9111409417988175496, 0.9401539645359766606) ) ) 
 REPRESENTATION_ITEM ( '' )  SURFACE ( )  );
#14081 = CARTESIAN_POINT ( 'NONE',  ( -82.39999999999999147, -33.20624999877097139, 96.53589838486223584 ) ) ;
#14082 = CARTESIAN_POINT ( 'NONE',  ( -79.39999999999999147, -30.26249999999999929, 101.7320508075688537 ) ) ;
#14083 = CARTESIAN_POINT ( 'NONE',  ( 94.79999999999991189, -3.000000000000000000, 150.0000000000000000 ) ) ;
#14084 = LINE ( 'NONE', #1978, #1648 ) ;
#14085 = CARTESIAN_POINT ( 'NONE',  ( 79.64356964374998427, -32.76562499938548711, -101.5914258081833879 ) ) ;
#14086 = CARTESIAN_POINT ( 'NONE',  ( 80.90000000000000568, -33.75000000000000000, 102.5980762113533018 ) ) ;
#14087 = CARTESIAN_POINT ( 'NONE',  ( -82.39999999999999147, -32.72812499938548569, 103.1828516163667899 ) ) ;
#14088 = CARTESIAN_POINT ( 'NONE',  ( 113.0000000000000142, 15.19999999999994955, 50.00000000000001421 ) ) ;
#14089 = ORIENTED_EDGE ( 'NONE', *, *, #770, .T. ) ;
#14090 =( NAMED_UNIT ( * ) PLANE_ANGLE_UNIT ( ) SI_UNIT ( $, .RADIAN. ) );
#14091 = CARTESIAN_POINT ( 'NONE',  ( -79.39999999999999147, -33.86250000000000426, 101.7320508075688537 ) ) ;
#14092 = LINE ( 'NONE', #5123, #13316 ) ;
#14093 = CARTESIAN_POINT ( 'NONE',  ( 231.2217848218749339, -32.57812499938548001, 97.61286128772489690 ) ) ;
#14094 = CARTESIAN_POINT ( 'NONE',  ( -81.02178482187500208, -34.45312499938548711, 97.61286128772489690 ) ) ;
#14095 = CARTESIAN_POINT ( 'NONE',  ( 235.3564303562499447, -30.81562499938547717, -50.00000000000011369 ) ) ;
#14096 = CARTESIAN_POINT ( 'NONE',  ( -79.39999999999999147, -32.06250000000000000, 101.7320508075688537 ) ) ;
#14097 = VERTEX_POINT ( 'NONE', #12862 ) ;
#14098 = CARTESIAN_POINT ( 'NONE',  ( -81.79008970393689992, -35.00000000000000000, -97.30603528924575585 ) ) ;
#14099 = DIRECTION ( 'NONE',  ( 1.000000000000000000, 0.000000000000000000, 0.000000000000000000 ) ) ;
#14100 = CARTESIAN_POINT ( 'NONE',  ( 79.64356964375001269, -33.55312499938548854, 98.40857419181659793 ) ) ;
#14101 = VECTOR ( 'NONE', #7019, 1000.000000000000000 ) ;
#14102 = VECTOR ( 'NONE', #17984, 1000.000000000000000 ) ;
#14103 = CARTESIAN_POINT ( 'NONE',  ( 83.20384757729337366, -32.55134618820330417, -103.0000000000000000 ) ) ;
#14104 = CARTESIAN_POINT ( 'NONE',  ( -79.64356964374999848, -33.62812499938548427, 99.99999999999998579 ) ) ;
#14105 = CARTESIAN_POINT ( 'NONE',  ( 94.79999999999995453, -32.00000000000000000, 150.0000000000000000 ) ) ;
#14106 = CARTESIAN_POINT ( 'NONE',  ( 79.64356964374999848, -32.61562499938548854, 99.99999999999998579 ) ) ;
#14107 = CARTESIAN_POINT ( 'NONE',  ( 83.77821517812500929, -31.22812499938548569, -97.61286128772489690 ) ) ;
#14108 = CARTESIAN_POINT ( 'NONE',  ( 232.5999999999999375, -32.50312499938547717, -53.18285161636690361 ) ) ;
#14109 = CARTESIAN_POINT ( 'NONE',  ( -85.15643035625001289, -34.30312499938548854, 99.99999999999998579 ) ) ;
#14110 = CARTESIAN_POINT ( 'NONE',  ( -83.77821517812500929, -31.56562499938548427, -102.3871387122750889 ) ) ;
#14111 = ORIENTED_EDGE ( 'NONE', *, *, #12736, .F. ) ;
#14112 = CARTESIAN_POINT ( 'NONE',  ( 82.39999999999999147, -33.51562499938548001, 103.1828516163667899 ) ) ;
#14113 = CIRCLE ( 'NONE', #405, 6.000000000000005329 ) ;
#14114 = CARTESIAN_POINT ( 'NONE',  ( -81.02178482187500208, -32.09062499938548285, 97.61286128772489690 ) ) ;
#14115 = CARTESIAN_POINT ( 'NONE',  ( -85.15643035625001289, -33.40312499938548285, 99.99999999999998579 ) ) ;
#14116 = CARTESIAN_POINT ( 'NONE',  ( 82.40000000000000568, -30.00000000000000355, 99.99999999999998579 ) ) ;
#14117 = VERTEX_POINT ( 'NONE', #18833 ) ;
#14118 = CARTESIAN_POINT ( 'NONE',  ( -79.39999999999999147, -34.31250000000000000, -98.26794919243113213 ) ) ;
#14119 = DIRECTION ( 'NONE',  ( 0.000000000000000000, 0.000000000000000000, 1.000000000000000000 ) ) ;
#14120 = CARTESIAN_POINT ( 'NONE',  ( 231.0429922824658320, -35.00000000000000711, -52.57249805494185324 ) ) ;
#14121 = PLANE ( 'NONE',  #7966 ) ;
#14122 = EDGE_CURVE ( 'NONE', #11560, #5607, #12717, .T. ) ;
#14123 = CARTESIAN_POINT ( 'NONE',  ( 235.3564303562499447, -32.20312499938548001, 101.5914258081833879 ) ) ;
#14124 = CARTESIAN_POINT ( 'NONE',  ( -85.40000000000000568, -35.31018749875867258, 101.7320508075688679 ) ) ;
#14125 = CARTESIAN_POINT ( 'NONE',  ( -79.64356964374999848, -34.97812499938548569, 99.99999999999998579 ) ) ;
#14126 = CARTESIAN_POINT ( 'NONE',  ( 79.39999999999999147, -32.83124999877097139, -98.26794919243110371 ) ) ;
#14127 = CARTESIAN_POINT ( 'NONE',  ( 83.20395887649176814, -35.00000000000002132, 97.36341917746361219 ) ) ;
#14128 = CARTESIAN_POINT ( 'NONE',  ( 79.64356964374999848, -30.92812499938548498, 99.99999999999998579 ) ) ;
#14129 = AXIS2_PLACEMENT_3D ( 'NONE', #7718, #13288, #17895 ) ;
#14130 =( BOUNDED_CURVE ( )  B_SPLINE_CURVE ( 2, ( #7831, #4910, #3434, #9385, #6469, #12421, #15744, #9686, #2452 ),
 .UNSPECIFIED., .F., .F. ) 
 B_SPLINE_CURVE_WITH_KNOTS ( ( 3, 2, 2, 2, 3 ),
 ( 0.5625000000000001110, 0.5694444444444444198, 0.5833333333333333703, 0.5972222222222222099, 0.6041666666666667407 ),
 .UNSPECIFIED. ) 
 CURVE ( )  GEOMETRIC_REPRESENTATION_ITEM ( )  RATIONAL_B_SPLINE_CURVE ( ( 0.9330127018922194093, 0.9330127018922204085, 1.000000000000000000, 0.8660254037844387076, 1.000000000000000000, 0.8660254037844387076, 1.000000000000000000, 0.9330127018922187432, 0.9330127018922192983 ) ) 
 REPRESENTATION_ITEM ( '' )  );
#14131 = ADVANCED_BREP_SHAPE_REPRESENTATION ( '', ( #7516, #10540 ), #5560 ) ;
#14132 = DIRECTION ( 'NONE',  ( 0.000000000000000000, 0.000000000000000000, -1.000000000000000000 ) ) ;
#14133 = CARTESIAN_POINT ( 'NONE',  ( 82.39999999999999147, -31.94062499938548427, -103.1828516163667899 ) ) ;
#14134 = CARTESIAN_POINT ( 'NONE',  ( 230.3018593135002448, -35.00052333152935802, 98.07164593887567605 ) ) ;
#14135 = ORIENTED_EDGE ( 'NONE', *, *, #9187, .F. ) ;
#14136 = CARTESIAN_POINT ( 'NONE',  ( 80.90000000000000568, -31.14374999877097139, 97.40192378864668399 ) ) ;
#14137 = SHAPE_DEFINITION_REPRESENTATION ( #18565, #406 ) ;
#14138 = ADVANCED_FACE ( 'NONE', ( #2498 ), #763, .F. ) ;
#14139 = CARTESIAN_POINT ( 'NONE',  ( 231.2217848218749339, -31.67812499938547788, 97.61286128772489690 ) ) ;
#14140 = CARTESIAN_POINT ( 'NONE',  ( 231.2217848218749339, -32.12812499938547717, -52.38713871227520968 ) ) ;
#14141 = EDGE_CURVE ( 'NONE', #16515, #5564, #8095, .T. ) ;
#14142 = CARTESIAN_POINT ( 'NONE',  ( -85.15643035625001289, -32.84062499938548285, 99.99999999999998579 ) ) ;
#14143 = DIRECTION ( 'NONE',  ( -1.000000000000000000, 0.000000000000000000, 0.000000000000000000 ) ) ;
#14144 = ORIENTED_EDGE ( 'NONE', *, *, #8760, .T. ) ;
#14145 = ORIENTED_EDGE ( 'NONE', *, *, #7854, .T. ) ;
#14146 = CARTESIAN_POINT ( 'NONE',  ( -79.64356964375001269, -32.12812499938548427, -101.5914258081833879 ) ) ;
#14147 = EDGE_CURVE ( 'NONE', #14, #16006, #16597, .T. ) ;
#14148 = DIRECTION ( 'NONE',  ( -1.000000000000000000, 0.000000000000000000, 0.000000000000000000 ) ) ;
#14149 = ORIENTED_EDGE ( 'NONE', *, *, #458, .T. ) ;
#14150 = CARTESIAN_POINT ( 'NONE',  ( 83.77821517812500929, -32.87812499938548427, 97.61286128772489690 ) ) ;
#14151 = CARTESIAN_POINT ( 'NONE',  ( -79.39999999999999147, -34.25624999877096855, -98.26794919243113213 ) ) ;
#14152 = CARTESIAN_POINT ( 'NONE',  ( 83.90000000000000568, -34.57500000000000284, 102.5980762113533018 ) ) ;
#14153 = CARTESIAN_POINT ( 'NONE',  ( 105.1999999999999744, -4.999999999999976907, 150.0000000000000000 ) ) ;
#14154 = CARTESIAN_POINT ( 'NONE',  ( -82.39999999999999147, -31.85624999877097352, 96.53589838486223584 ) ) ;
#14155 = CARTESIAN_POINT ( 'NONE',  ( -79.39999999999999147, -33.73124999877096997, 98.26794919243110371 ) ) ;
#14156 = CARTESIAN_POINT ( 'NONE',  ( 83.65502553131049979, -34.99999999999999289, -102.4885329066889028 ) ) ;
#14157 = DIRECTION ( 'NONE',  ( -1.000000000000000000, 0.000000000000000000, -0.000000000000000000 ) ) ;
#14158 = EDGE_CURVE ( 'NONE', #16231, #17606, #4735, .T. ) ;
#14159 = CARTESIAN_POINT ( 'NONE',  ( 235.3140393761304665, -32.00000000000000000, 101.2782762865722361 ) ) ;
#14160 = CARTESIAN_POINT ( 'NONE',  ( 229.8435696437499303, -34.19062499938547717, 99.99999999999998579 ) ) ;
#14161 = ORIENTED_EDGE ( 'NONE', *, *, #6672, .T. ) ;
#14162 = CARTESIAN_POINT ( 'NONE',  ( 81.02178482187500208, -32.54062499938548569, -97.61286128772489690 ) ) ;
#14163 =( LENGTH_UNIT ( ) NAMED_UNIT ( * ) SI_UNIT ( .MILLI., .METRE. ) );
#14164 = DIRECTION ( 'NONE',  ( 0.000000000000000000, 0.000000000000000000, 1.000000000000000000 ) ) ;
#14165 = CARTESIAN_POINT ( 'NONE',  ( 231.0999999999999375, -30.46874999877096002, -52.59807621135342970 ) ) ;
#14166 = EDGE_LOOP ( 'NONE', ( #2809, #16170, #13512, #13384 ) ) ;
#14167 = CARTESIAN_POINT ( 'NONE',  ( -79.39999999999999147, -35.15624999877096712, 101.7320508075688537 ) ) ;
#14168 = CYLINDRICAL_SURFACE ( 'NONE', #6497, 3.000000000000002665 ) ;
#14169 = DIRECTION ( 'NONE',  ( 0.000000000000000000, -0.000000000000000000, -1.000000000000000000 ) ) ;
#14170 = EDGE_LOOP ( 'NONE', ( #1846, #3114, #6108, #13556 ) ) ;
#14171 = CARTESIAN_POINT ( 'NONE',  ( -85.15643035625001289, -30.14062499938548711, 99.99999999999998579 ) ) ;
#14172 = CARTESIAN_POINT ( 'NONE',  ( 4.104070371397485317, -2.023683613428366890, 3.505122836902509587 ) ) ;
#14173 = EDGE_LOOP ( 'NONE', ( #5161, #6779, #16803, #9904 ) ) ;
#14174 = CARTESIAN_POINT ( 'NONE',  ( 80.90000000000000568, -33.75000000000000000, -97.40192378864668399 ) ) ;
#14175 = EDGE_CURVE ( 'NONE', #804, #15440, #11778, .T. ) ;
#14176 = CARTESIAN_POINT ( 'NONE',  ( -81.02178482187500208, -34.90312499938548285, -102.3871387122750889 ) ) ;
#14177 = CARTESIAN_POINT ( 'NONE',  ( -80.90000000000000568, -35.04374999877096997, 97.40192378864668399 ) ) ;
#14178 = CARTESIAN_POINT ( 'NONE',  ( -80.90000000000000568, -30.60000000000000142, 97.40192378864668399 ) ) ;
#14179 = CARTESIAN_POINT ( 'NONE',  ( 83.90000000000000568, -32.32500000000000284, -97.40192378864668399 ) ) ;
#14180 = CARTESIAN_POINT ( 'NONE',  ( 229.8435696437499018, -35.11426555956767714, 98.99674139749697588 ) ) ;
#14181 = CARTESIAN_POINT ( 'NONE',  ( 231.7961524227065695, -32.10134618820329422, -47.00000000000011369 ) ) ;
#14182 = FACE_OUTER_BOUND ( 'NONE', #632, .T. ) ;
#14183 = CARTESIAN_POINT ( 'NONE',  ( -81.02178482187500208, -33.14062499938548711, 102.3871387122750889 ) ) ;
#14184 = CARTESIAN_POINT ( 'NONE',  ( 82.40000000000000568, -30.00000000000000355, -99.99999999999998579 ) ) ;
#14185 = VERTEX_POINT ( 'NONE', #13435 ) ;
#14186 = CARTESIAN_POINT ( 'NONE',  ( 231.0999999999999375, -34.57499999999999574, -52.59807621135342970 ) ) ;
#14187 = CARTESIAN_POINT ( 'NONE',  ( -82.40000000000000568, -30.00000000000000355, -103.0000000000000000 ) ) ;
#14188 = PRODUCT_DEFINITION_SHAPE ( 'NONE', 'NONE',  #19324 ) ;
#14189 = CARTESIAN_POINT ( 'NONE',  ( -82.40000000000001990, -33.88124999877096855, 103.0000000000000000 ) ) ;
#14190 = CARTESIAN_POINT ( 'NONE',  ( 235.3564303562499447, -32.31562499938547717, 101.5914258081833879 ) ) ;
#14191 = CARTESIAN_POINT ( 'NONE',  ( -79.64356964374999848, -33.62812499938548427, 99.99999999999998579 ) ) ;
#14192 = CARTESIAN_POINT ( 'NONE',  ( 229.8435696437499303, -30.14062499938548001, -50.00000000000011369 ) ) ;
#14193 = ORIENTED_EDGE ( 'NONE', *, *, #3870, .T. ) ;
#14194 = APPLICATION_CONTEXT ( 'automotive_design' ) ;
#14195 = CARTESIAN_POINT ( 'NONE',  ( 4.158921784487744411, 2.089935040870094074, 3.500000000000000444 ) ) ;
#14196 = CARTESIAN_POINT ( 'NONE',  ( 83.03192786677290371, -34.99999999999999289, 97.31096265645994947 ) ) ;
#14197 = CARTESIAN_POINT ( 'NONE',  ( 81.02178482187500208, -32.09062499938548285, 102.3871387122750889 ) ) ;
#14198 = VECTOR ( 'NONE', #15302, 1000.000000000000000 ) ;
#14199 = CARTESIAN_POINT ( 'NONE',  ( 230.9489134087919524, -32.00820041275123629, -52.22959632847759082 ) ) ;
#14200 = CARTESIAN_POINT ( 'NONE',  ( -82.39999999999999147, -32.84062499938548996, 103.1828516163667899 ) ) ;
#14201 = CARTESIAN_POINT ( 'NONE',  ( -81.02178482187500208, -32.20312499938548711, -102.3871387122750889 ) ) ;
#14202 = CARTESIAN_POINT ( 'NONE',  ( 85.15643035624999868, -32.80312499938548854, 98.40857419181659793 ) ) ;
#14203 = CARTESIAN_POINT ( 'NONE',  ( 79.64356964375001269, -35.01562499938548711, -101.5914258081833879 ) ) ;
#14204 = CARTESIAN_POINT ( 'NONE',  ( 235.3564303562499447, -33.10312499938547859, -48.40857419181671162 ) ) ;
#14205 = CARTESIAN_POINT ( 'NONE',  ( -84.05108659120801917, -32.00820041275124339, 97.77040367152252998 ) ) ;
#14206 = EDGE_LOOP ( 'NONE', ( #14043, #18392, #18441, #14919 ) ) ;
#14207 = CARTESIAN_POINT ( 'NONE',  ( 82.39999999999999147, -31.71562499938548640, 103.1828516163667899 ) ) ;
#14208 = CARTESIAN_POINT ( 'NONE',  ( 229.5999999999999375, -32.28749999999999432, 98.26794919243111792 ) ) ;
#14209 = CARTESIAN_POINT ( 'NONE',  ( -79.39999999999999147, -34.27499999999999858, 99.99999999999998579 ) ) ;
#14210 = CARTESIAN_POINT ( 'NONE',  ( -85.15643035624999868, -30.62812499938548427, 98.40857419181659793 ) ) ;
#14211 = CARTESIAN_POINT ( 'NONE',  ( -85.15643035624999868, -31.90312499938548285, 101.5914258081833879 ) ) ;
#14212 = LINE ( 'NONE', #2396, #9922 ) ;
#14213 = VERTEX_POINT ( 'NONE', #10220 ) ;
#14214 = CARTESIAN_POINT ( 'NONE',  ( -80.90000000000000568, -34.20000000000000284, -102.5980762113533018 ) ) ;
#14215 = CARTESIAN_POINT ( 'NONE',  ( 0.3461262719736147297, -4.658553426539303821, -3.671615880910379381 ) ) ;
#14216 = DIRECTION ( 'NONE',  ( -0.000000000000000000, -0.000000000000000000, -1.000000000000000000 ) ) ;
#14217 = CARTESIAN_POINT ( 'NONE',  ( 100.0000000000000000, 10.19999999999999218, -139.9999999999999716 ) ) ;
#14218 =( GEOMETRIC_REPRESENTATION_CONTEXT ( 3 ) GLOBAL_UNCERTAINTY_ASSIGNED_CONTEXT ( ( #13872 ) ) GLOBAL_UNIT_ASSIGNED_CONTEXT ( ( #7702, #12003, #16692 ) ) REPRESENTATION_CONTEXT ( 'NONE', 'WORKASPACE' ) );
#14219 = CARTESIAN_POINT ( 'NONE',  ( -82.40000000000000568, -34.78124999877096712, -96.99999999999998579 ) ) ;
#14220 = CARTESIAN_POINT ( 'NONE',  ( 83.90000000000000568, -34.06874999877096855, -97.40192378864668399 ) ) ;
#14221 = CARTESIAN_POINT ( 'NONE',  ( -82.39999999999999147, -33.43124999877097281, -96.99999999999998579 ) ) ;
#14222 = CARTESIAN_POINT ( 'NONE',  ( -83.20384757729335945, -33.05759618943233136, 102.9999999999999858 ) ) ;
#14223 = CARTESIAN_POINT ( 'NONE',  ( 85.15643035625001289, -30.70312499938548711, 99.99999999999998579 ) ) ;
#14224 = LINE ( 'NONE', #9838, #16179 ) ;
#14225 = CARTESIAN_POINT ( 'NONE',  ( -85.40000000000000568, -32.66250000000000142, -98.26794919243111792 ) ) ;
#14226 = CARTESIAN_POINT ( 'NONE',  ( 83.77821517812500929, -30.62812499938548783, -102.3871387122750889 ) ) ;
#14227 = LINE ( 'NONE', #17465, #8026 ) ;
#14228 = EDGE_CURVE ( 'NONE', #11694, #5568, #2979, .T. ) ;
#14229 = EDGE_LOOP ( 'NONE', ( #13982, #13590, #16416, #8020 ) ) ;
#14230 = CARTESIAN_POINT ( 'NONE',  ( 79.39999999999999147, -30.61874999877096926, 99.99999999999998579 ) ) ;
#14231 = CARTESIAN_POINT ( 'NONE',  ( 232.5999999999999375, -35.09062499938547575, 103.1828516163667899 ) ) ;
#14232 = CARTESIAN_POINT ( 'NONE',  ( 235.3564303562499447, -32.76562499938548001, -48.40857419181671162 ) ) ;
#14233 = ADVANCED_FACE ( 'NONE', ( #4357 ), #66, .F. ) ;
#14234 = EDGE_CURVE ( 'NONE', #8302, #14497, #6019, .T. ) ;
#14235 = CARTESIAN_POINT ( 'NONE',  ( -79.64356964375001269, -33.02812499938548285, 98.40857419181659793 ) ) ;
#14236 = CARTESIAN_POINT ( 'NONE',  ( -83.65502553130849606, -35.00000000000002842, -97.51146709331030138 ) ) ;
#14237 = VERTEX_POINT ( 'NONE', #1621 ) ;
#14238 = CARTESIAN_POINT ( 'NONE',  ( -81.02178482187500208, -30.89062499938548711, -97.61286128772489690 ) ) ;
#14239 = LINE ( 'NONE', #11221, #713 ) ;
#14240 = VERTEX_POINT ( 'NONE', #14799 ) ;
#14241 = CARTESIAN_POINT ( 'NONE',  ( 85.15643035625001289, -32.46562499938548996, 98.40857419181659793 ) ) ;
#14242 = CARTESIAN_POINT ( 'NONE',  ( -81.02178482187500208, -30.55312499938548854, -97.61286128772489690 ) ) ;
#14243 =( BOUNDED_CURVE ( )  B_SPLINE_CURVE ( 2, ( #10519, #13252, #16487, #7393, #8950, #19126, #12079, #14918, #2994 ),
 .UNSPECIFIED., .F., .F. ) 
 B_SPLINE_CURVE_WITH_KNOTS ( ( 3, 2, 2, 2, 3 ),
 ( 0.6041666666666666297, 0.6111111111111111605, 0.6250000000000000000, 0.6388888888888888395, 0.6458333333333333703 ),
 .UNSPECIFIED. ) 
 CURVE ( )  GEOMETRIC_REPRESENTATION_ITEM ( )  RATIONAL_B_SPLINE_CURVE ( ( 0.9330127018922192983, 0.9330127018922187432, 1.000000000000000000, 0.8660254037844387076, 1.000000000000000000, 0.8660254037844387076, 1.000000000000000000, 0.9330127018922187432, 0.9330127018922192983 ) ) 
 REPRESENTATION_ITEM ( '' )  );
#14244 = CARTESIAN_POINT ( 'NONE',  ( 79.39999999999999147, -34.76250000000000284, 98.26794919243113213 ) ) ;
#14245 = CARTESIAN_POINT ( 'NONE',  ( -80.85389467647070205, -34.99999999999999289, 97.51091559654260266 ) ) ;
#14246 = CARTESIAN_POINT ( 'NONE',  ( -80.90000000000000568, -32.04374999877096997, 102.5980762113533018 ) ) ;
#14247 = CARTESIAN_POINT ( 'NONE',  ( -83.90000000000000568, -35.26874999877097139, 102.5980762113533018 ) ) ;
#14248 = CARTESIAN_POINT ( 'NONE',  ( -79.64356964374998427, -33.55312499938548854, -98.40857419181659793 ) ) ;
#14249 = PRODUCT_DEFINITION_FORMATION_WITH_SPECIFIED_SOURCE ( 'ANY', '', #12793, .NOT_KNOWN. ) ;
#14250 = EDGE_CURVE ( 'NONE', #3130, #15577, #14697, .T. ) ;
#14251 = EDGE_CURVE ( 'NONE', #12317, #16053, #9615, .T. ) ;
#14252 = CARTESIAN_POINT ( 'NONE',  ( 94.79999999999995453, -29.80000000000000071, -150.0000000000000000 ) ) ;
#14253 = VECTOR ( 'NONE', #5285, 1000.000000000000000 ) ;
#14254 = CARTESIAN_POINT ( 'NONE',  ( 231.0999999999999375, -30.07499999999999574, 97.40192378864668399 ) ) ;
#14255 = ORIENTED_EDGE ( 'NONE', *, *, #14754, .T. ) ;
#14256 = CARTESIAN_POINT ( 'NONE',  ( 82.39999999999999147, -33.62812499938548427, -103.1828516163667899 ) ) ;
#14257 = CARTESIAN_POINT ( 'NONE',  ( -83.77821517812500929, -34.71562499938548285, -102.3871387122750889 ) ) ;
#14258 = CARTESIAN_POINT ( 'NONE',  ( 235.5999999999999375, -31.96874999877096002, -50.00000000000011369 ) ) ;
#14259 = VERTEX_POINT ( 'NONE', #1336 ) ;
#14260 = CARTESIAN_POINT ( 'NONE',  ( -81.71550957129744575, -35.02336225948853610, 96.93108911813138207 ) ) ;
#14261 = CARTESIAN_POINT ( 'NONE',  ( -79.64356964374998427, -30.77812499938548285, 98.40857419181659793 ) ) ;
#14262 = CARTESIAN_POINT ( 'NONE',  ( -1.747541505913277282, 3.837784562140256650, -3.503702292528906526 ) ) ;
#14263 = ORIENTED_EDGE ( 'NONE', *, *, #8428, .F. ) ;
#14264 = CARTESIAN_POINT ( 'NONE',  ( -82.39999999999999147, -32.98124999877096286, -96.99999999999998579 ) ) ;
#14265 = CARTESIAN_POINT ( 'NONE',  ( -80.90000000000000568, -33.84374999877096712, 102.5980762113533018 ) ) ;
#14266 = ORIENTED_EDGE ( 'NONE', *, *, #11468, .F. ) ;
#14267 =( NAMED_UNIT ( * ) PLANE_ANGLE_UNIT ( ) SI_UNIT ( $, .RADIAN. ) );
#14268 = CARTESIAN_POINT ( 'NONE',  ( 79.39999999999999147, -31.98750000000000071, -98.26794919243110371 ) ) ;
#14269 = CARTESIAN_POINT ( 'NONE',  ( -82.40000000000000568, -30.00000000000000355, 99.99999999999998579 ) ) ;
#14270 = CONICAL_SURFACE ( 'NONE', #1791, 2.055000000000000160, 0.7853981633974439491 ) ;
#14271 = MECHANICAL_DESIGN_GEOMETRIC_PRESENTATION_REPRESENTATION (  '', ( #17080 ), #3676 ) ;
#14272 = CARTESIAN_POINT ( 'NONE',  ( -83.77821517812500929, -32.12812499938548427, 97.61286128772489690 ) ) ;
#14273 = CARTESIAN_POINT ( 'NONE',  ( -83.90000000000000568, -34.12106250001229313, 97.40192378864668399 ) ) ;
#14274 = UNCERTAINTY_MEASURE_WITH_UNIT (LENGTH_MEASURE( 1.000000000000000082E-05 ), #533, 'distance_accuracy_value', 'NONE');
#14275 = CARTESIAN_POINT ( 'NONE',  ( 4.630153689607048761, 0.000000000000000000, -5.371010071662833063 ) ) ;
#14276 = CARTESIAN_POINT ( 'NONE',  ( 232.8516854624778887, -31.99999999999997868, -52.85844335754083545 ) ) ;
#14277 = CARTESIAN_POINT ( 'NONE',  ( 84.28136653320183314, -32.00000000000000711, 102.0145392219077394 ) ) ;
#14278 = VECTOR ( 'NONE', #3354, 1000.000000000000000 ) ;
#14279 = FACE_OUTER_BOUND ( 'NONE', #8688, .T. ) ;
#14280 = CARTESIAN_POINT ( 'NONE',  ( -85.15643035625001289, -32.39062499938548711, 99.99999999999998579 ) ) ;
#14281 = DIRECTION ( 'NONE',  ( 0.000000000000000000, 0.000000000000000000, 1.000000000000000000 ) ) ;
#14282 = ORIENTED_EDGE ( 'NONE', *, *, #10777, .T. ) ;
#14283 = CARTESIAN_POINT ( 'NONE',  ( 229.5999999999999659, -34.97364041986482874, -51.09190422181774949 ) ) ;
#14284 = CARTESIAN_POINT ( 'NONE',  ( 232.5999999999999091, -34.10624999877096286, 96.99999999999998579 ) ) ;
#14285 = CIRCLE ( 'NONE', #15220, 5.199999999999996625 ) ;
#14286 = CARTESIAN_POINT ( 'NONE',  ( 83.32052461991715120, -34.98323688327303671, 102.9326364780328760 ) ) ;
#14287 = DIRECTION ( 'NONE',  ( -1.000000000000000000, 0.000000000000000000, -0.000000000000000000 ) ) ;
#14288 = CARTESIAN_POINT ( 'NONE',  ( -85.15643035624999868, -34.71562499938548285, 101.5914258081833879 ) ) ;
#14289 = CARTESIAN_POINT ( 'NONE',  ( 233.9782151781249411, -31.34062499938548285, -47.61286128772501769 ) ) ;
#14290 = ORIENTED_EDGE ( 'NONE', *, *, #11902, .T. ) ;
#14291 = CARTESIAN_POINT ( 'NONE',  ( -81.94448577231695197, -35.00123065787786913, 97.01484129690837221 ) ) ;
#14292 = AXIS2_PLACEMENT_3D ( 'NONE', #4958, #13825, #10901 ) ;
#14293 = EDGE_CURVE ( 'NONE', #2327, #11976, #18602, .T. ) ;
#14294 = CARTESIAN_POINT ( 'NONE',  ( -84.51155491706698797, -35.14114833091483803, 98.22820877610629964 ) ) ;
#14295 = CARTESIAN_POINT ( 'NONE',  ( -79.39999999999999147, -33.78750000000000853, -101.7320508075688963 ) ) ;
#14296 = CARTESIAN_POINT ( 'NONE',  ( 82.39999999999999147, -32.27812499938548285, 96.81714838363319586 ) ) ;
#14297 = DIRECTION ( 'NONE',  ( 1.000000000000000000, 0.000000000000000000, 4.625929269271481378E-15 ) ) ;
#14298 = CARTESIAN_POINT ( 'NONE',  ( 231.2217848218749339, -32.76562499938548001, -47.61286128772501769 ) ) ;
#14299 = CARTESIAN_POINT ( 'NONE',  ( -82.39999999999999147, -34.41562499938548569, 96.81714838363319586 ) ) ;
#14300 = CARTESIAN_POINT ( 'NONE',  ( -85.15643035625001289, -33.44062499938548427, -101.5914258081833879 ) ) ;
#14301 = CARTESIAN_POINT ( 'NONE',  ( 82.39999999999999147, -32.72812499938548569, 96.81714838363319586 ) ) ;
#14302 = CARTESIAN_POINT ( 'NONE',  ( 85.15643035625001289, -33.40312499938548285, -99.99999999999998579 ) ) ;
#14303 = CARTESIAN_POINT ( 'NONE',  ( 235.3564303562499447, -33.96562499938547575, -50.00000000000011369 ) ) ;
#14304 = CARTESIAN_POINT ( 'NONE',  ( -79.64356964374999848, -33.51562499938548711, 99.99999999999998579 ) ) ;
#14305 = CARTESIAN_POINT ( 'NONE',  ( 79.64356964375001269, -30.32812499938548711, -98.40857419181659793 ) ) ;
#14306 = ORIENTED_EDGE ( 'NONE', *, *, #12466, .F. ) ;
#14307 = DIRECTION ( 'NONE',  ( -0.000000000000000000, -1.000000000000000000, -0.000000000000000000 ) ) ;
#14308 = CARTESIAN_POINT ( 'NONE',  ( 4.236525694536557474, -2.416953475386482530, -3.751298745799839462 ) ) ;
#14309 = CARTESIAN_POINT ( 'NONE',  ( -80.90000000000000568, -33.00000000000000000, 102.5980762113533018 ) ) ;
#14310 = CARTESIAN_POINT ( 'NONE',  ( -83.77821517812500929, -30.21562499938548285, 97.61286128772489690 ) ) ;
#14311 = CARTESIAN_POINT ( 'NONE',  ( -85.15643035624999868, -31.45312499938548356, 101.5914258081833879 ) ) ;
#14312 = DIRECTION ( 'NONE',  ( 0.000000000000000000, 0.000000000000000000, -1.000000000000000000 ) ) ;
#14313 = EDGE_LOOP ( 'NONE', ( #11574, #10161, #7419, #1653 ) ) ;
#14314 = CARTESIAN_POINT ( 'NONE',  ( -85.40000000000000568, -33.56250000000000000, -98.26794919243111792 ) ) ;
#14315 = CARTESIAN_POINT ( 'NONE',  ( 231.7961524227065695, -34.35134618820329422, -47.00000000000009948 ) ) ;
#14316 = LINE ( 'NONE', #955, #17949 ) ;
#14317 = CARTESIAN_POINT ( 'NONE',  ( -80.90000000000000568, -30.74606250001229313, 102.5980762113533018 ) ) ;
#14318 = CARTESIAN_POINT ( 'NONE',  ( 4.158806965674307854, 4.075748668183980961, 0.05940377217583493047 ) ) ;
#14319 = CARTESIAN_POINT ( 'NONE',  ( -3.974357786152442180E-13, 4.796734841935204052, -3.721909803043259579 ) ) ;
#14320 = PLANE ( 'NONE',  #5724 ) ;
#14321 = CARTESIAN_POINT ( 'NONE',  ( -83.90000000000000568, -33.52499999999999858, 102.5980762113533018 ) ) ;
#14322 = CARTESIAN_POINT ( 'NONE',  ( -82.39999999999999147, -32.98124999877096286, -96.99999999999998579 ) ) ;
#14323 = CARTESIAN_POINT ( 'NONE',  ( 235.3140393761304665, -32.00000000000000000, 101.2782762865722361 ) ) ;
#14324 = EDGE_CURVE ( 'NONE', #16645, #4020, #11230, .T. ) ;
#14325 = CARTESIAN_POINT ( 'NONE',  ( 94.79999999999984084, 0.000000000000000000, -150.0000000000000000 ) ) ;
#14326 = CARTESIAN_POINT ( 'NONE',  ( 79.64356964374999848, -33.17812499938548854, -99.99999999999998579 ) ) ;
#14327 = ORIENTED_EDGE ( 'NONE', *, *, #18568, .T. ) ;
#14328 = CARTESIAN_POINT ( 'NONE',  ( 85.40000000000000568, -31.33124999877096428, 101.7320508075688679 ) ) ;
#14329 = ITEM_DEFINED_TRANSFORMATION ( 'NONE', 'NONE', #5203,  #10540 ) ;
#14330 = CARTESIAN_POINT ( 'NONE',  ( 232.5999999999999375, -33.74062499938548143, 103.1828516163667899 ) ) ;
#14331 = CARTESIAN_POINT ( 'NONE',  ( 235.3564303562499447, -33.66562499938548569, -48.40857419181671162 ) ) ;
#14332 = CARTESIAN_POINT ( 'NONE',  ( -82.39999999999999147, -34.75312499938549138, 96.81714838363319586 ) ) ;
#14333 = CARTESIAN_POINT ( 'NONE',  ( 232.5999999999999375, -32.81249999999999289, -53.00000000000011369 ) ) ;
#14334 = ORIENTED_EDGE ( 'NONE', *, *, #7911, .T. ) ;
#14335 = CARTESIAN_POINT ( 'NONE',  ( -83.77821517812500929, -31.86562499938548498, -97.61286128772489690 ) ) ;
#14336 = LINE ( 'NONE', #17570, #7858 ) ;
#14337 = ORIENTED_EDGE ( 'NONE', *, *, #3251, .F. ) ;
#14338 = CARTESIAN_POINT ( 'NONE',  ( 81.02178482187500208, -32.65312499938548996, 102.3871387122750889 ) ) ;
#14339 = CARTESIAN_POINT ( 'NONE',  ( -85.15643035625001289, -32.05312499938548854, -99.99999999999998579 ) ) ;
#14340 = CARTESIAN_POINT ( 'NONE',  ( -83.90000000000000568, -30.46874999877096712, -102.5980762113533018 ) ) ;
#14341 = CARTESIAN_POINT ( 'NONE',  ( 80.90000000000000568, -34.74374999877097281, -102.5980762113533018 ) ) ;
#14342 = CARTESIAN_POINT ( 'NONE',  ( -79.39999999999999147, -34.70624999877097139, 101.7320508075688537 ) ) ;
#14343 = CARTESIAN_POINT ( 'NONE',  ( -83.77821517812500929, -30.77812499938548640, 97.61286128772489690 ) ) ;
#14344 = CARTESIAN_POINT ( 'NONE',  ( -83.77821517812500929, -32.91562499938547859, -102.3871387122750889 ) ) ;
#14345 = EDGE_CURVE ( 'NONE', #15086, #14185, #13620, .T. ) ;
#14346 = PRODUCT_DEFINITION_SHAPE ( 'NONE', 'NONE',  #19329 ) ;
#14347 = DIRECTION ( 'NONE',  ( -0.000000000000000000, -1.000000000000000000, -0.000000000000000000 ) ) ;
#14348 = CARTESIAN_POINT ( 'NONE',  ( 80.90000000000000568, -30.69374999877097210, -102.5980762113533018 ) ) ;
#14349 = CARTESIAN_POINT ( 'NONE',  ( 232.5999999999999375, -30.56250000000000000, 96.53589838486223584 ) ) ;
#14350 = VERTEX_POINT ( 'NONE', #4806 ) ;
#14351 = CARTESIAN_POINT ( 'NONE',  ( 85.15643035625001289, -33.25312499938548427, -101.5914258081833879 ) ) ;
#14352 = CARTESIAN_POINT ( 'NONE',  ( 229.5999999999999375, -33.58124999877096428, 98.26794919243111792 ) ) ;
#14353 = CARTESIAN_POINT ( 'NONE',  ( 231.0999999999999375, -31.81874999877096144, -52.59807621135342970 ) ) ;
#14354 = VERTEX_POINT ( 'NONE', #7264 ) ;
#14355 = DIRECTION ( 'NONE',  ( -1.000000000000000000, 0.000000000000000000, 0.000000000000000000 ) ) ;
#14356 = CARTESIAN_POINT ( 'NONE',  ( -83.77821517812500929, -31.11562499938548498, 97.61286128772489690 ) ) ;
#14357 = LINE ( 'NONE', #6664, #11920 ) ;
#14358 = ORIENTED_EDGE ( 'NONE', *, *, #15091, .T. ) ;
#14359 = CARTESIAN_POINT ( 'NONE',  ( 111.5987303322250597, 7.969082163015149156, -134.2945615375061550 ) ) ;
#14361 = ADVANCED_FACE ( 'NONE', ( #1315 ), #4338, .T. ) ;
#14360 = CARTESIAN_POINT ( 'NONE',  ( 4.142654963991909689, -2.035398498734318995, 3.525413613457260009 ) ) ;
#14362 = VERTEX_POINT ( 'NONE', #7817 ) ;
#14363 =( LENGTH_UNIT ( ) NAMED_UNIT ( * ) SI_UNIT ( .MILLI., .METRE. ) );
#14364 = CARTESIAN_POINT ( 'NONE',  ( 82.39999999999999147, -33.93750000000000000, -103.4641016151377499 ) ) ;
#14365 = CARTESIAN_POINT ( 'NONE',  ( -4.000000000000000000, 2.309401076758498483, -3.433295621305379353 ) ) ;
#14366 = CARTESIAN_POINT ( 'NONE',  ( -85.15643035624999868, -31.56562499938548427, 101.5914258081833879 ) ) ;
#14367 = CARTESIAN_POINT ( 'NONE',  ( -79.39999999999999147, -32.06250000000000000, 101.7320508075688537 ) ) ;
#14368 = CARTESIAN_POINT ( 'NONE',  ( -82.39999999999999147, -34.83749999999999858, -97.00000000000000000 ) ) ;
#14369 = FILL_AREA_STYLE_COLOUR ( '', #1946 ) ;
#14370 = ADVANCED_FACE ( 'NONE', ( #5806 ), #14579, .F. ) ;
#14371 = CARTESIAN_POINT ( 'NONE',  ( 82.40000000000000568, -34.10624999877096997, 102.9999999999999858 ) ) ;
#14372 = FACE_OUTER_BOUND ( 'NONE', #12048, .T. ) ;
#14373 = CARTESIAN_POINT ( 'NONE',  ( 84.70388354820681798, -35.00002705695767702, 101.9214814096700934 ) ) ;
#14374 = CARTESIAN_POINT ( 'NONE',  ( 232.5999999999999375, -34.78124999877096002, -47.00000000000011369 ) ) ;
#14375 = ORIENTED_EDGE ( 'NONE', *, *, #11858, .F. ) ;
#14376 = CARTESIAN_POINT ( 'NONE',  ( 235.5999999999999943, -34.31249999999999289, -48.26794919243124582 ) ) ;
#14377 = CYLINDRICAL_SURFACE ( 'NONE', #14574, 3.000000000000002665 ) ;
#14378 = CARTESIAN_POINT ( 'NONE',  ( -82.40000000000000568, -30.00000000000000355, 96.99999999999998579 ) ) ;
#14379 = CARTESIAN_POINT ( 'NONE',  ( 235.3564303562499447, -34.07812499938548001, 99.99999999999998579 ) ) ;
#14380 = CARTESIAN_POINT ( 'NONE',  ( -83.77821517812500929, -33.02812499938548285, 97.61286128772489690 ) ) ;
#14381 = CARTESIAN_POINT ( 'NONE',  ( 233.9782151781249411, -31.64062499938547646, -52.38713871227520968 ) ) ;
#14382 = EDGE_CURVE ( 'NONE', #13090, #3915, #5248, .T. ) ;
#14383 = ORIENTED_EDGE ( 'NONE', *, *, #5896, .F. ) ;
#14384 = CARTESIAN_POINT ( 'NONE',  ( -85.15643035625001289, -34.19062499938548427, 99.99999999999998579 ) ) ;
#14385 = CARTESIAN_POINT ( 'NONE',  ( 85.40000000000000568, -32.23124999877096997, -98.26794919243111792 ) ) ;
#14386 = CARTESIAN_POINT ( 'NONE',  ( 79.64356964375001269, -34.00312499938549138, 98.40857419181659793 ) ) ;
#14387 = DIRECTION ( 'NONE',  ( -0.000000000000000000, -1.000000000000000000, -0.000000000000000000 ) ) ;
#14388 = CARTESIAN_POINT ( 'NONE',  ( 111.0000000000000000, 6.932050807568743700, -145.0319487353994532 ) ) ;
#14389 = CARTESIAN_POINT ( 'NONE',  ( -83.77821517812500929, -33.47812499938548569, 97.61286128772489690 ) ) ;
#14390 = CARTESIAN_POINT ( 'NONE',  ( -85.15643035625001289, -34.30312499938548854, -99.99999999999998579 ) ) ;
#14391 = CARTESIAN_POINT ( 'NONE',  ( 79.64356964375001269, -31.75312499938548427, 98.40857419181659793 ) ) ;
#14392 = CARTESIAN_POINT ( 'NONE',  ( 79.64356964375001269, -33.59062499938548285, -98.40857419181659793 ) ) ;
#14393 = EDGE_CURVE ( 'NONE', #15931, #4595, #17626, .T. ) ;
#14394 = CARTESIAN_POINT ( 'NONE',  ( 235.3564303562499447, -34.00312499938547717, -48.40857419181671162 ) ) ;
#14395 = CARTESIAN_POINT ( 'NONE',  ( -85.15643035625001289, -33.77812499938548285, 98.40857419181659793 ) ) ;
#14396 = CARTESIAN_POINT ( 'NONE',  ( 79.64356964375001269, -31.75312499938548427, -101.5914258081833879 ) ) ;
#14397 = ORIENTED_EDGE ( 'NONE', *, *, #14008, .F. ) ;
#14398 = DIRECTION ( 'NONE',  ( 0.000000000000000000, 0.000000000000000000, -1.000000000000000000 ) ) ;
#14399 = DIRECTION ( 'NONE',  ( 1.000000000000000000, -1.586032892321652285E-15, 0.000000000000000000 ) ) ;
#14400 = CARTESIAN_POINT ( 'NONE',  ( -79.39999999999999147, -33.41250000000000142, 101.7320508075688537 ) ) ;
#14401 = CARTESIAN_POINT ( 'NONE',  ( -79.64356964375001269, -33.47812499938547859, 98.40857419181659793 ) ) ;
#14402 = CARTESIAN_POINT ( 'NONE',  ( -82.39999999999999147, -30.92812499938548143, 103.1828516163667899 ) ) ;
#14403 = LINE ( 'NONE', #6905, #4628 ) ;
#14404 = AXIS2_PLACEMENT_3D ( 'NONE', #7952, #4937, #17140 ) ;
#14405 = CARTESIAN_POINT ( 'NONE',  ( 235.3564303562499447, -32.61562499938548143, 99.99999999999998579 ) ) ;
#14406 = DIRECTION ( 'NONE',  ( 1.000000000000000000, 0.000000000000000000, -0.000000000000000000 ) ) ;
#14407 = LINE ( 'NONE', #12951, #13904 ) ;
#14408 = ADVANCED_FACE ( 'NONE', ( #5713 ), #4145, .F. ) ;
#14409 = LINE ( 'NONE', #1236, #5175 ) ;
#14410 = CARTESIAN_POINT ( 'NONE',  ( 85.40000000000000568, -33.95624999877097139, -101.7320508075688821 ) ) ;
#14411 = LINE ( 'NONE', #8553, #1344 ) ;
#14412 = CARTESIAN_POINT ( 'NONE',  ( 244.7999999999999545, -32.00000000000000000, -100.0000000000000000 ) ) ;
#14413 = CARTESIAN_POINT ( 'NONE',  ( -83.90000000000000568, -33.01874999877097139, -97.40192378864668399 ) ) ;
#14414 = CARTESIAN_POINT ( 'NONE',  ( 233.4038475772933339, -32.06115380933863435, 103.0000000000000000 ) ) ;
#14415 = CARTESIAN_POINT ( 'NONE',  ( -83.20384757729335945, -32.60759618943233562, -96.99999999999997158 ) ) ;
#14416 = CARTESIAN_POINT ( 'NONE',  ( 83.77821517812500929, -33.47812499938548569, -97.61286128772489690 ) ) ;
#14417 = FACE_OUTER_BOUND ( 'NONE', #8879, .T. ) ;
#14418 = PRESENTATION_LAYER_ASSIGNMENT (  '', '', ( #18805 ) ) ;
#14419 = CIRCLE ( 'NONE', #2270, 2.100000000000000089 ) ;
#14420 = ORIENTED_EDGE ( 'NONE', *, *, #2788, .T. ) ;
#14421 = CARTESIAN_POINT ( 'NONE',  ( 82.39999999999999147, -34.33124999877097139, 96.53589838486223584 ) ) ;
#14422 = CONTEXT_DEPENDENT_SHAPE_REPRESENTATION ( #3580, #4064 ) ;
#14423 = CARTESIAN_POINT ( 'NONE',  ( 233.0319854768594041, -35.00000000000000000, -47.27181766474440394 ) ) ;
#14424 = CARTESIAN_POINT ( 'NONE',  ( 235.3564303562499447, -33.21562499938548285, -48.40857419181671162 ) ) ;
#14425 = CARTESIAN_POINT ( 'NONE',  ( -79.64356964375001269, -34.82812499938548711, 98.40857419181659793 ) ) ;
#14426 = CARTESIAN_POINT ( 'NONE',  ( 99.99999999999998579, 0.000000000000000000, 150.0000000000000000 ) ) ;
#14427 = ORIENTED_EDGE ( 'NONE', *, *, #11525, .T. ) ;
#14428 = CARTESIAN_POINT ( 'NONE',  ( -85.15643035625001289, -34.19062499938548427, -99.99999999999998579 ) ) ;
#14429 = CARTESIAN_POINT ( 'NONE',  ( 85.40000000000000568, -33.18750000000000000, 101.7320508075688821 ) ) ;
#14430 = ORIENTED_EDGE ( 'NONE', *, *, #9640, .T. ) ;
#14431 = CARTESIAN_POINT ( 'NONE',  ( 85.15643035625001289, -32.54062499938548569, 101.5914258081833879 ) ) ;
#14432 = CARTESIAN_POINT ( 'NONE',  ( -83.77821517812500929, -31.67812499938548498, -102.3871387122750889 ) ) ;
#14433 = CIRCLE ( 'NONE', #7582, 6.000000000000005329 ) ;
#14434 = CARTESIAN_POINT ( 'NONE',  ( 83.90000000000000568, -33.67500000000000426, 102.5980762113533018 ) ) ;
#14435 = CARTESIAN_POINT ( 'NONE',  ( -83.90000000000000568, -35.26874999877097139, 102.5980762113533018 ) ) ;
#14436 = CARTESIAN_POINT ( 'NONE',  ( -82.39999999999999147, -31.94062499938548427, 103.1828516163667899 ) ) ;
#14437 = CYLINDRICAL_SURFACE ( 'NONE', #18207, 3.000000000000009770 ) ;
#14438 = B_SPLINE_CURVE_WITH_KNOTS ( 'NONE', 3,
 ( #4427, #9300, #16445, #10582, #237, #43, #7745, #15264, #1690, #3055, #7547, #17817, #7838, #342, #13792, #11945, #13505, #12238 ),
 .UNSPECIFIED., .F., .F.,
 ( 4, 2, 2, 2, 2, 2, 2, 2, 4 ),
 ( 0.000000000000000000, 0.0007106627595359221467, 0.001421325519071844293, 0.002131988278607766657, 0.002842651038143688587, 0.003553313797679610517, 0.004263976557215533314, 0.004974639316751455244, 0.005685302076287377174 ),
 .UNSPECIFIED. ) ;
#14439 = CARTESIAN_POINT ( 'NONE',  ( -80.90000000000000568, -34.29374999877096997, -97.40192378864668399 ) ) ;
#14440 = CARTESIAN_POINT ( 'NONE',  ( 85.40000000000000568, -32.23124999877096997, -98.26794919243111792 ) ) ;
#14441 = CARTESIAN_POINT ( 'NONE',  ( 229.5999999999999375, -31.38749999999999218, 98.26794919243111792 ) ) ;
#14442 = EDGE_LOOP ( 'NONE', ( #10596, #6029, #748, #13789 ) ) ;
#14443 = CARTESIAN_POINT ( 'NONE',  ( 113.0000000000000000, 10.39615242270649276, -134.0032071715735640 ) ) ;
#14444 = SHAPE_REPRESENTATION_RELATIONSHIP ( 'NONE' , 'NONE' ,  #9634, #10882 ) ;
#14445 = CARTESIAN_POINT ( 'NONE',  ( 235.5999999999999943, -32.45624999877096428, 101.7320508075688537 ) ) ;
#14446 = CARTESIAN_POINT ( 'NONE',  ( 235.5999999999999943, -30.65624999877095647, -48.26794919243124582 ) ) ;
#14447 = CARTESIAN_POINT ( 'NONE',  ( 231.7961524227065695, -32.73615380933862440, 96.99999999999995737 ) ) ;
#14448 = CARTESIAN_POINT ( 'NONE',  ( -79.64356964374998427, -30.85312499938548569, 101.5914258081833879 ) ) ;
#14449 = VERTEX_POINT ( 'NONE', #4703 ) ;
#14450 = ORIENTED_EDGE ( 'NONE', *, *, #2183, .F. ) ;
#14451 = CARTESIAN_POINT ( 'NONE',  ( -81.59615242270662350, -31.87634618820330701, 97.00000000000000000 ) ) ;
#14452 = LINE ( 'NONE', #16128, #15044 ) ;
#14453 = VERTEX_POINT ( 'NONE', #15049 ) ;
#14454 = CARTESIAN_POINT ( 'NONE',  ( 85.40000000000000568, -33.60000000000000142, -99.99999999999998579 ) ) ;
#14455 = CARTESIAN_POINT ( 'NONE',  ( 83.52979456739228681, -32.00000000000000000, -102.5803447510191972 ) ) ;
#14456 = CARTESIAN_POINT ( 'NONE',  ( -82.39999999999999147, -30.59062499938548640, 103.1828516163667899 ) ) ;
#14457 = CARTESIAN_POINT ( 'NONE',  ( -79.39999999999999147, -31.53750000000000497, 98.26794919243110371 ) ) ;
#14458 = CARTESIAN_POINT ( 'NONE',  ( 234.1461053235293548, -35.00000000000002132, -52.48908440345743998 ) ) ;
#14459 = PRESENTATION_STYLE_ASSIGNMENT (( #17124 ) ) ;
#14460 = CARTESIAN_POINT ( 'NONE',  ( 232.5999999999999091, -32.08124999877096428, -47.00000000000011369 ) ) ;
#14461 = CARTESIAN_POINT ( 'NONE',  ( -0.6666666666666666297, -4.233901974057276973, -3.300726591567087365 ) ) ;
#14462 = CARTESIAN_POINT ( 'NONE',  ( 0.2174200650117547873, 3.876582599186211731, 0.2855619784720684895 ) ) ;
#14463 = CYLINDRICAL_SURFACE ( 'NONE', #12082, 2.649999999999985700 ) ;
#14464 = VERTEX_POINT ( 'NONE', #16617 ) ;
#14465 = CARTESIAN_POINT ( 'NONE',  ( -85.15643035625001289, -30.14062499938548711, -99.99999999999998579 ) ) ;
#14466 = CARTESIAN_POINT ( 'NONE',  ( -82.40000000000000568, -30.00000000000000355, -96.99999999999998579 ) ) ;
#14467 = EDGE_CURVE ( 'NONE', #6637, #11529, #8626, .T. ) ;
#14468 = SHAPE_REPRESENTATION ( 'MAS-172', ( #12987, #6770, #215, #5813, #11430, #16727, #2688, #13912, #10492, #13606, #12676, #2373, #2068, #5203, #7682, #17679 ), #4881 ) ;
#14469 = CARTESIAN_POINT ( 'NONE',  ( 83.90000000000000568, -34.81874999877096855, 97.40192378864668399 ) ) ;
#14470 = CARTESIAN_POINT ( 'NONE',  ( 231.2217848218749339, -34.37812499938547717, 97.61286128772489690 ) ) ;
#14471 = CARTESIAN_POINT ( 'NONE',  ( -85.15643035624999868, -33.44062499938548427, 98.40857419181659793 ) ) ;
#14472 = FACE_OUTER_BOUND ( 'NONE', #10894, .T. ) ;
#14473 = CARTESIAN_POINT ( 'NONE',  ( 229.8435696437499018, -35.22676555956767430, -51.00325860250310939 ) ) ;
#14474 = ADVANCED_FACE ( 'NONE', ( #1672, #16161 ), #2772, .T. ) ;
#14475 = ORIENTED_EDGE ( 'NONE', *, *, #6616, .F. ) ;
#14476 = CARTESIAN_POINT ( 'NONE',  ( -81.02178482187500208, -33.59062499938548285, 102.3871387122750889 ) ) ;
#14477 = CARTESIAN_POINT ( 'NONE',  ( -82.39999999999999147, -30.73124999877096641, 103.4641016151377499 ) ) ;
#14478 = CARTESIAN_POINT ( 'NONE',  ( 82.39999999999999147, -34.07812499938548711, 96.81714838363319586 ) ) ;
#14479 = DIRECTION ( 'NONE',  ( -1.000000000000000000, -0.000000000000000000, -0.000000000000000000 ) ) ;
#14480 = CARTESIAN_POINT ( 'NONE',  ( 229.8435696437499871, -30.55312499938547788, 101.5914258081833879 ) ) ;
#14481 = CARTESIAN_POINT ( 'NONE',  ( 83.20384757729335945, -32.73615380933863150, -96.99999999999998579 ) ) ;
#14482 = CARTESIAN_POINT ( 'NONE',  ( -82.39999999999999147, -33.74062499938548854, 103.1828516163667899 ) ) ;
#14483 = CARTESIAN_POINT ( 'NONE',  ( -82.39999999999999147, -33.06562499938548427, -103.1828516163667899 ) ) ;
#14484 = CARTESIAN_POINT ( 'NONE',  ( 82.39999999999999147, -33.20624999877097849, -97.00000000000000000 ) ) ;
#14485 = ADVANCED_FACE ( 'NONE', ( #15145 ), #15538, .F. ) ;
#14486 = CARTESIAN_POINT ( 'NONE',  ( 79.64356964374999848, -34.52812499938548285, -99.99999999999998579 ) ) ;
#14487 = CARTESIAN_POINT ( 'NONE',  ( 232.5999999999999375, -34.07812499938548001, -46.81714838363331666 ) ) ;
#14488 = CARTESIAN_POINT ( 'NONE',  ( -82.39999999999999147, -33.85312499938548569, 96.81714838363319586 ) ) ;
#14489 = CARTESIAN_POINT ( 'NONE',  ( 3.958476099524242731, -1.406653531810796443, -3.500000000000000000 ) ) ;
#14490 = EDGE_CURVE ( 'NONE', #12222, #4900, #4098, .T. ) ;
#14491 = ORIENTED_EDGE ( 'NONE', *, *, #9393, .T. ) ;
#14492 = CARTESIAN_POINT ( 'NONE',  ( 85.15643035625001289, -34.30312499938548854, 99.99999999999998579 ) ) ;
#14493 = CARTESIAN_POINT ( 'NONE',  ( -82.39999999999999147, -32.58750000000000568, 102.9999999999999858 ) ) ;
#14494 = CARTESIAN_POINT ( 'NONE',  ( -82.39999999999999147, -32.58750000000000568, 103.4641016151377499 ) ) ;
#14495 = CARTESIAN_POINT ( 'NONE',  ( -82.39999999999999147, -33.62812499938549138, 103.1828516163667899 ) ) ;
#14496 = CARTESIAN_POINT ( 'NONE',  ( -85.15643035624999868, -31.07812499938548356, 98.40857419181659793 ) ) ;
#14497 = VERTEX_POINT ( 'NONE', #3800 ) ;
#14498 = CARTESIAN_POINT ( 'NONE',  ( -82.40000000000000568, -33.71249999999998437, -102.9999999999999858 ) ) ;
#14499 = MECHANICAL_DESIGN_GEOMETRIC_PRESENTATION_REPRESENTATION (  '', ( #806 ), #13571 ) ;
#14500 = CARTESIAN_POINT ( 'NONE',  ( 235.3564303562499447, -32.12812499938547717, 98.40857419181659793 ) ) ;
#14501 = CARTESIAN_POINT ( 'NONE',  ( -94.79999999999999716, -32.00000000000000000, 150.0000000000000000 ) ) ;
#14502 = DIRECTION ( 'NONE',  ( -1.000000000000000000, 1.387778780781445676E-15, 2.407412430484046130E-31 ) ) ;
#14503 = CARTESIAN_POINT ( 'NONE',  ( -79.39999999999999147, -34.72500000000000142, 99.99999999999998579 ) ) ;
#14504 = CARTESIAN_POINT ( 'NONE',  ( -79.39999999999999147, -32.86874999877097281, 99.99999999999998579 ) ) ;
#14505 = CARTESIAN_POINT ( 'NONE',  ( -82.39999999999999147, -30.25312499938548783, 96.81714838363319586 ) ) ;
#14506 = CARTESIAN_POINT ( 'NONE',  ( 84.67508262029681987, -32.00000000000000000, 98.43364869553350616 ) ) ;
#14507 = DIRECTION ( 'NONE',  ( 0.000000000000000000, 0.000000000000000000, -1.000000000000000000 ) ) ;
#14508 = LINE ( 'NONE', #1144, #10254 ) ;
#14509 = FACE_OUTER_BOUND ( 'NONE', #5956, .T. ) ;
#14510 = CARTESIAN_POINT ( 'NONE',  ( 81.02178482187500208, -34.45312499938548711, -97.61286128772489690 ) ) ;
#14511 = CARTESIAN_POINT ( 'NONE',  ( 231.0999999999999375, -34.12499999999999289, 97.40192378864668399 ) ) ;
#14512 = AXIS2_PLACEMENT_3D ( 'NONE', #3285, #13930, #10999 ) ;
#14513 = VERTEX_POINT ( 'NONE', #889 ) ;
#14514 =( BOUNDED_CURVE ( )  B_SPLINE_CURVE ( 2, ( #15058, #32, #6083, #9004, #16337, #11934, #4324, #133, #10376 ),
 .UNSPECIFIED., .F., .F. ) 
 B_SPLINE_CURVE_WITH_KNOTS ( ( 3, 2, 2, 2, 3 ),
 ( 0.7708333333333332593, 0.7777777777777777901, 0.7916666666666666297, 0.8055555555555555802, 0.8125000000000000000 ),
 .UNSPECIFIED. ) 
 CURVE ( )  GEOMETRIC_REPRESENTATION_ITEM ( )  RATIONAL_B_SPLINE_CURVE ( ( 0.9330127018922192983, 0.9330127018922187432, 1.000000000000000000, 0.8660254037844387076, 1.000000000000000000, 0.8660254037844387076, 1.000000000000000000, 0.9330127018922194093, 0.9330127018922194093 ) ) 
 REPRESENTATION_ITEM ( '' )  );
#14515 = CARTESIAN_POINT ( 'NONE',  ( 80.90000000000000568, -32.34374999877096712, 102.5980762113533018 ) ) ;
#14516 = CONTEXT_DEPENDENT_SHAPE_REPRESENTATION ( #10580, #9996 ) ;
#14517 = CARTESIAN_POINT ( 'NONE',  ( 230.4884461346514968, -35.25364837475780178, 98.22820752270799005 ) ) ;
#14518 = ADVANCED_FACE ( 'NONE', ( #12409 ), #4896, .F. ) ;
#14519 = CARTESIAN_POINT ( 'NONE',  ( 0.000000000000000000, 0.000000000000000000, 0.000000000000000000 ) ) ;
#14520 = DIRECTION ( 'NONE',  ( 0.000000000000000000, 0.000000000000000000, -1.000000000000000000 ) ) ;
#14521 = CARTESIAN_POINT ( 'NONE',  ( -83.20395887649183919, -35.00000000000001421, -97.36341917746362640 ) ) ;
#14522 = ORIENTED_EDGE ( 'NONE', *, *, #15000, .T. ) ;
#14523 = CARTESIAN_POINT ( 'NONE',  ( -83.77821517812500929, -34.11562499938548854, -97.61286128772489690 ) ) ;
#14524 = DIRECTION ( 'NONE',  ( 0.000000000000000000, 0.000000000000000000, -1.000000000000000000 ) ) ;
#14525 = VERTEX_POINT ( 'NONE', #3515 ) ;
#14526 = DIRECTION ( 'NONE',  ( 0.000000000000000000, 0.000000000000000000, 1.000000000000000000 ) ) ;
#14527 = EDGE_CURVE ( 'NONE', #16633, #1370, #11347, .T. ) ;
#14528 = CARTESIAN_POINT ( 'NONE',  ( -82.39999999999999147, -32.16562499938549280, -103.1828516163667899 ) ) ;
#14529 = PRODUCT_RELATED_PRODUCT_CATEGORY ( 'part', '', ( #791 ) ) ;
#14530 = CARTESIAN_POINT ( 'NONE',  ( -80.90000000000000568, -31.14374999877097139, -97.40192378864668399 ) ) ;
#14531 = CARTESIAN_POINT ( 'NONE',  ( -79.69416654173919312, -34.99999999999999289, 100.6274906301336216 ) ) ;
#14532 = CARTESIAN_POINT ( 'NONE',  ( -79.39999999999999147, -30.58518749875867826, 98.26794919243110371 ) ) ;
#14533 = CARTESIAN_POINT ( 'NONE',  ( -79.64356964375001269, -31.41562499938548569, 101.5914258081833879 ) ) ;
#14534 = CARTESIAN_POINT ( 'NONE',  ( -79.64356964374999848, -32.61562499938548854, -99.99999999999998579 ) ) ;
#14535 = CARTESIAN_POINT ( 'NONE',  ( 231.0999999999999375, -32.17499999999999716, -47.40192378864679768 ) ) ;
#14536 = CARTESIAN_POINT ( 'NONE',  ( 83.90000000000000568, -31.66874999877096997, -102.5980762113533018 ) ) ;
#14537 = CARTESIAN_POINT ( 'NONE',  ( 235.5999999999999943, -31.16249999999999432, 101.7320508075688537 ) ) ;
#14538 = ORIENTED_EDGE ( 'NONE', *, *, #14234, .T. ) ;
#14539 = LINE ( 'NONE', #4007, #4142 ) ;
#14540 = CARTESIAN_POINT ( 'NONE',  ( 231.0999999999999375, -33.61874999877096570, 97.40192378864668399 ) ) ;
#14541 = CARTESIAN_POINT ( 'NONE',  ( 235.5999999999999375, -31.06874999877096144, -50.00000000000011369 ) ) ;
#14542 = CARTESIAN_POINT ( 'NONE',  ( 232.5999999999999091, -34.38749999999999574, 102.9999999999999858 ) ) ;
#14543 = CARTESIAN_POINT ( 'NONE',  ( 113.0000000000000000, 10.39615242270649453, -149.9961509411812415 ) ) ;
#14544 = ORIENTED_EDGE ( 'NONE', *, *, #16870, .T. ) ;
#14545 = ORIENTED_EDGE ( 'NONE', *, *, #10564, .F. ) ;
#14546 = CARTESIAN_POINT ( 'NONE',  ( -82.39999999999999147, -34.83749999999999858, 103.0000000000000000 ) ) ;
#14547 = DIRECTION ( 'NONE',  ( -0.000000000000000000, -1.000000000000000000, -0.000000000000000000 ) ) ;
#14548 = ORIENTED_EDGE ( 'NONE', *, *, #1020, .F. ) ;
#14549 = CARTESIAN_POINT ( 'NONE',  ( -82.65333140691201663, -34.99995246259153703, -102.9892844631211943 ) ) ;
#14550 = CARTESIAN_POINT ( 'NONE',  ( 83.90000000000000568, -32.32500000000000284, -97.40192378864668399 ) ) ;
#14551 = CARTESIAN_POINT ( 'NONE',  ( -4.000000000000000888, -1.539600717839011201, -3.300726591567081591 ) ) ;
#14552 = CARTESIAN_POINT ( 'NONE',  ( -82.39999999999999147, -31.04062499938548569, 103.1828516163667899 ) ) ;
#14553 = CARTESIAN_POINT ( 'NONE',  ( -83.90000000000000568, -30.97500000000000142, 97.40192378864668399 ) ) ;
#14554 = DIRECTION ( 'NONE',  ( 0.000000000000000000, -1.000000000000000000, 0.000000000000000000 ) ) ;
#14555 = CARTESIAN_POINT ( 'NONE',  ( 85.15643035625001289, -34.60312499938548569, 98.40857419181659793 ) ) ;
#14556 = CARTESIAN_POINT ( 'NONE',  ( -6.259644161404860030E-16, -4.618802153517027165, -3.433295621305388234 ) ) ;
#14557 = DIRECTION ( 'NONE',  ( -0.000000000000000000, -0.000000000000000000, -1.000000000000000000 ) ) ;
#14558 = CARTESIAN_POINT ( 'NONE',  ( 231.2217848218749339, -31.11562499938547788, 97.61286128772489690 ) ) ;
#14559 = ORIENTED_EDGE ( 'NONE', *, *, #13471, .T. ) ;
#14560 = AXIS2_PLACEMENT_3D ( 'NONE', #10706, #9234, #1816 ) ;
#14561 = SURFACE_STYLE_FILL_AREA ( #4125 ) ;
#14562 = CARTESIAN_POINT ( 'NONE',  ( -79.64356964375001269, -30.40312499938548285, -98.40857419181659793 ) ) ;
#14563 = B_SPLINE_CURVE_WITH_KNOTS ( 'NONE', 3,
 ( #4495, #10450, #18969, #1184, #7520, #12204, #13853, #12111, #16608, #13476, #9173, #8982, #4797, #4888, #7808, #1850 ),
 .UNSPECIFIED., .F., .F.,
 ( 4, 3, 3, 3, 3, 4 ),
 ( -2.111273352579591097E-06, 0.000000000000000000, 3.519286887794390245E-05, 7.191842652046569998E-05, 0.0001049868727088885950, 0.0001382836236814613518 ),
 .UNSPECIFIED. ) ;
#14564 = CARTESIAN_POINT ( 'NONE',  ( 234.6787480663870156, -35.00000000000000711, 97.97655282300767965 ) ) ;
#14565 = CARTESIAN_POINT ( 'NONE',  ( 99.99999999999995737, -21.80000000000003268, -139.9999999999999716 ) ) ;
#14566 = CARTESIAN_POINT ( 'NONE',  ( 235.3564303562499447, -34.04062499938548569, 98.40857419181659793 ) ) ;
#14567 = CARTESIAN_POINT ( 'NONE',  ( -82.39999999999999147, -30.25312499938548783, 96.81714838363319586 ) ) ;
#14568 = CARTESIAN_POINT ( 'NONE',  ( 231.2217848218749339, -32.91562499938547148, -52.38713871227520968 ) ) ;
#14569 = VECTOR ( 'NONE', #10612, 1000.000000000000000 ) ;
#14570 = EDGE_LOOP ( 'NONE', ( #8979, #7843 ) ) ;
#14571 = CARTESIAN_POINT ( 'NONE',  ( -83.77821517812500929, -32.91562499938547859, 97.61286128772489690 ) ) ;
#14572 = DIRECTION ( 'NONE',  ( -0.000000000000000000, -0.000000000000000000, -1.000000000000000000 ) ) ;
#14573 = CARTESIAN_POINT ( 'NONE',  ( 79.39999999999999147, -30.22500000000000142, 99.99999999999998579 ) ) ;
#14574 = AXIS2_PLACEMENT_3D ( 'NONE', #12920, #4221, #5511 ) ;
#14575 = B_SPLINE_CURVE_WITH_KNOTS ( 'NONE', 3,
 ( #17699, #7049, #10276, #18783, #16238, #2843, #13008, #14276, #912, #18977, #6871, #11351, #2461, #12913, #18881, #317, #5881, #17991 ),
 .UNSPECIFIED., .F., .F.,
 ( 4, 2, 2, 2, 2, 2, 2, 2, 4 ),
 ( 0.000000000000000000, 0.0007089252359835750269, 0.001417850471967150054, 0.002126775707950724972, 0.002835700943934300108, 0.003544626179917875243, 0.004253551415901449945, 0.004962476651885025514, 0.005671401887868600215 ),
 .UNSPECIFIED. ) ;
#14576 = CARTESIAN_POINT ( 'NONE',  ( -82.40000000000000568, -30.00000000000000355, 99.99999999999998579 ) ) ;
#14577 = CARTESIAN_POINT ( 'NONE',  ( 235.3564303562499447, -32.16562499938547859, 99.99999999999998579 ) ) ;
#14578 = CARTESIAN_POINT ( 'NONE',  ( 235.3564303562499447, -32.57812499938548001, -51.59142580818350154 ) ) ;
#14579 = CYLINDRICAL_SURFACE ( 'NONE', #11762, 3.000000000000002665 ) ;
#14580 = AXIS2_PLACEMENT_3D ( 'NONE', #17056, #9428, #15396 ) ;
#14581 = CARTESIAN_POINT ( 'NONE',  ( -79.64356964374999848, -33.62812499938548427, -99.99999999999998579 ) ) ;
#14582 = CARTESIAN_POINT ( 'NONE',  ( 81.02178482187500208, -33.89062499938548711, 102.3871387122750889 ) ) ;
#14583 = EDGE_CURVE ( 'NONE', #10357, #677, #8299, .T. ) ;
#14584 =( BOUNDED_CURVE ( )  B_SPLINE_CURVE ( 2, ( #11736, #16042, #3037, #4318, #5978, #19074, #11834, #7154, #16241 ),
 .UNSPECIFIED., .F., .F. ) 
 B_SPLINE_CURVE_WITH_KNOTS ( ( 3, 2, 2, 2, 3 ),
 ( 0.8125000000000000000, 0.8194444444444444198, 0.8333333333333333703, 0.8472222222222222099, 0.8541666666666665186 ),
 .UNSPECIFIED. ) 
 CURVE ( )  GEOMETRIC_REPRESENTATION_ITEM ( )  RATIONAL_B_SPLINE_CURVE ( ( 0.9330127018922194093, 0.9330127018922194093, 1.000000000000000000, 0.8660254037844387076, 1.000000000000000000, 0.8660254037844387076, 1.000000000000000000, 0.9330127018922209636, 0.9330127018922194093 ) ) 
 REPRESENTATION_ITEM ( '' )  );
#14585 =( GEOMETRIC_REPRESENTATION_CONTEXT ( 3 ) GLOBAL_UNCERTAINTY_ASSIGNED_CONTEXT ( ( #15274 ) ) GLOBAL_UNIT_ASSIGNED_CONTEXT ( ( #16243, #7156, #10370 ) ) REPRESENTATION_CONTEXT ( 'NONE', 'WORKASPACE' ) );
#14586 = EDGE_CURVE ( 'NONE', #15758, #11141, #17970, .T. ) ;
#14587 = CARTESIAN_POINT ( 'NONE',  ( 85.15643035624999868, -35.22676555956768141, -98.99674139749697588 ) ) ;
#14588 = CARTESIAN_POINT ( 'NONE',  ( 231.0999999999999375, -30.07499999999999574, -52.59807621135342970 ) ) ;
#14589 = CARTESIAN_POINT ( 'NONE',  ( -83.77821517812500929, -33.36562499938548854, 97.61286128772489690 ) ) ;
#14590 = CARTESIAN_POINT ( 'NONE',  ( 4.158921444904714271, -2.089933220600049157, -3.500000000000000000 ) ) ;
#14591 = VERTEX_POINT ( 'NONE', #12500 ) ;
#14592 = FACE_OUTER_BOUND ( 'NONE', #18654, .T. ) ;
#14593 = CARTESIAN_POINT ( 'NONE',  ( 235.5999999999999943, -34.18124999877096570, -51.73205080756900287 ) ) ;
#14594 = CARTESIAN_POINT ( 'NONE',  ( -80.90000000000000568, -33.89999999999999858, 102.5980762113533018 ) ) ;
#14595 = CARTESIAN_POINT ( 'NONE',  ( -82.39999999999999147, -32.72812499938548569, 103.1828516163667899 ) ) ;
#14596 = ORIENTED_EDGE ( 'NONE', *, *, #1136, .F. ) ;
#14597 = CARTESIAN_POINT ( 'NONE',  ( 232.5999999999999375, -29.99999999999999645, -50.00000000000011369 ) ) ;
#14598 = VECTOR ( 'NONE', #16814, 1000.000000000000000 ) ;
#14599 = ADVANCED_FACE ( 'NONE', ( #5090, #18279 ), #2336, .T. ) ;
#14600 = VECTOR ( 'NONE', #5502, 1000.000000000000000 ) ;
#14601 = EDGE_CURVE ( 'NONE', #17445, #18941, #16998, .T. ) ;
#14602 = CARTESIAN_POINT ( 'NONE',  ( 231.2217848218749339, -33.66562499938547859, 102.3871387122750889 ) ) ;
#14603 = CARTESIAN_POINT ( 'NONE',  ( 80.48808202378427268, -35.00000000000000711, -97.80480077079582202 ) ) ;
#14604 = CARTESIAN_POINT ( 'NONE',  ( -83.90000000000000568, -30.52106250001229526, 97.40192378864668399 ) ) ;
#14605 = CARTESIAN_POINT ( 'NONE',  ( 3.950241966887534151, 3.393956070637314859, -1.121495646999261186 ) ) ;
#14606 = CARTESIAN_POINT ( 'NONE',  ( 235.0681666926251410, -32.00000000000000000, -48.31447495408071546 ) ) ;
#14607 = CARTESIAN_POINT ( 'NONE',  ( -82.39999999999999147, -31.37812499938548427, 103.1828516163667899 ) ) ;
#14608 = CARTESIAN_POINT ( 'NONE',  ( -85.40000000000000568, -32.64374999877097139, 99.99999999999998579 ) ) ;
#14609 = CARTESIAN_POINT ( 'NONE',  ( 79.64356964375001269, -33.59062499938548285, 101.5914258081833879 ) ) ;
#14610 = EDGE_CURVE ( 'NONE', #3788, #11625, #19263, .T. ) ;
#14611 = CARTESIAN_POINT ( 'NONE',  ( -99.99999999999998579, -3.000000000000000000, -150.0000000000000000 ) ) ;
#14612 = CARTESIAN_POINT ( 'NONE',  ( 0.000000000000000000, 0.000000000000000000, 0.000000000000000000 ) ) ;
#14613 = CARTESIAN_POINT ( 'NONE',  ( 85.15643035625001289, -34.30312499938548854, -99.99999999999998579 ) ) ;
#14614 = ORIENTED_EDGE ( 'NONE', *, *, #12687, .F. ) ;
#14615 = CARTESIAN_POINT ( 'NONE',  ( 79.39999999999999147, -32.90624999877096712, 98.26794919243113213 ) ) ;
#14616 = ITEM_DEFINED_TRANSFORMATION ( 'NONE', 'NONE', #7682,  #10540 ) ;
#14617 = CARTESIAN_POINT ( 'NONE',  ( 235.2218879900010506, -35.00000000000000000, -49.14934632385183022 ) ) ;
#14618 = PLANE ( 'NONE',  #7418 ) ;
#14619 = CARTESIAN_POINT ( 'NONE',  ( 110.9999999999999574, -21.80000000000003268, -139.9999999999999716 ) ) ;
#14620 = FACE_OUTER_BOUND ( 'NONE', #18679, .T. ) ;
#14621 = VERTEX_POINT ( 'NONE', #15730 ) ;
#14622 = CARTESIAN_POINT ( 'NONE',  ( -85.15643035624999868, -33.25312499938548427, -98.40857419181659793 ) ) ;
#14623 = CARTESIAN_POINT ( 'NONE',  ( 94.79999999999995453, -32.00000000000000000, 150.0000000000000000 ) ) ;
#14624 = ORIENTED_EDGE ( 'NONE', *, *, #10245, .F. ) ;
#14625 = CARTESIAN_POINT ( 'NONE',  ( -85.40000000000000568, -32.19374999877096855, 99.99999999999998579 ) ) ;
#14626 = CARTESIAN_POINT ( 'NONE',  ( -79.39999999999999147, -35.15624999877096712, -98.26794919243113213 ) ) ;
#14627 = DIRECTION ( 'NONE',  ( 0.000000000000000000, -0.000000000000000000, -1.000000000000000000 ) ) ;
#14628 = CARTESIAN_POINT ( 'NONE',  ( -79.39999999999999147, -31.10624999877097352, -98.26794919243113213 ) ) ;
#14629 = CARTESIAN_POINT ( 'NONE',  ( 229.8435696437499303, -31.15312499938548285, 99.99999999999998579 ) ) ;
#14630 = CARTESIAN_POINT ( 'NONE',  ( -85.40000000000000568, -33.99374999877097281, 99.99999999999998579 ) ) ;
#14631 = CARTESIAN_POINT ( 'NONE',  ( -83.77821517812500929, -31.07812499938548711, 102.3871387122750889 ) ) ;
#14632 = CARTESIAN_POINT ( 'NONE',  ( -83.77821517812500929, -33.36562499938548854, -102.3871387122750889 ) ) ;
#14633 = CARTESIAN_POINT ( 'NONE',  ( 79.39999999999999147, -32.47500000000000142, -99.99999999999998579 ) ) ;
#14634 =( BOUNDED_CURVE ( )  B_SPLINE_CURVE ( 2, ( #12905, #5197, #2454, #2255, #18775, #11144, #14265, #619, #714 ),
 .UNSPECIFIED., .F., .F. ) 
 B_SPLINE_CURVE_WITH_KNOTS ( ( 3, 2, 2, 2, 3 ),
 ( 0.6041666666666665186, 0.6111111111111111605, 0.6250000000000000000, 0.6388888888888888395, 0.6458333333333333703 ),
 .UNSPECIFIED. ) 
 CURVE ( )  GEOMETRIC_REPRESENTATION_ITEM ( )  RATIONAL_B_SPLINE_CURVE ( ( 0.9330127018922194093, 0.9330127018922177440, 1.000000000000000000, 0.8660254037844387076, 1.000000000000000000, 0.8660254037844387076, 1.000000000000000000, 0.9330127018922187432, 0.9330127018922192983 ) ) 
 REPRESENTATION_ITEM ( '' )  );
#14635 = CARTESIAN_POINT ( 'NONE',  ( 82.40000000000000568, -34.38749999999999574, -102.9999999999999858 ) ) ;
#14636 = CARTESIAN_POINT ( 'NONE',  ( 82.39999999999999147, -31.85624999877097352, -96.53589838486223584 ) ) ;
#14637 = CARTESIAN_POINT ( 'NONE',  ( 232.5999999999999375, -31.01249999999999218, 96.53589838486223584 ) ) ;
#14638 = ORIENTED_EDGE ( 'NONE', *, *, #10234, .T. ) ;
#14639 = FACE_OUTER_BOUND ( 'NONE', #13294, .T. ) ;
#14640 = EDGE_CURVE ( 'NONE', #5496, #11985, #6364, .T. ) ;
#14641 = CARTESIAN_POINT ( 'NONE',  ( 232.5999999999999375, -33.43124999877096570, 103.4641016151377499 ) ) ;
#14642 = CARTESIAN_POINT ( 'NONE',  ( 232.5999999999999375, -33.43124999877096570, -46.53589838486234953 ) ) ;
#14643 = CARTESIAN_POINT ( 'NONE',  ( -85.15643035625001289, -31.07812499938548356, 98.40857419181659793 ) ) ;
#14644 = ORIENTED_EDGE ( 'NONE', *, *, #8170, .F. ) ;
#14645 = VERTEX_POINT ( 'NONE', #16114 ) ;
#14646 = LINE ( 'NONE', #7228, #13506 ) ;
#14647 = CARTESIAN_POINT ( 'NONE',  ( -82.40000000000000568, -50.00000000000000000, 107.5000000000000142 ) ) ;
#14648 = FACE_OUTER_BOUND ( 'NONE', #3227, .T. ) ;
#14649 = VERTEX_POINT ( 'NONE', #2822 ) ;
#14650 = CYLINDRICAL_SURFACE ( 'NONE', #9842, 6.000000000000005329 ) ;
#14651 = CARTESIAN_POINT ( 'NONE',  ( 79.39999999999999147, -34.76250000000000284, -101.7320508075688537 ) ) ;
#14652 = DIRECTION ( 'NONE',  ( 0.000000000000000000, 0.000000000000000000, -1.000000000000000000 ) ) ;
#14653 = PRODUCT_DEFINITION ( 'UNKNOWN', '', #10805, #6317 ) ;
#14654 = CARTESIAN_POINT ( 'NONE',  ( -79.64356964375001269, -31.34062499938548640, 98.40857419181659793 ) ) ;
#14655 = CARTESIAN_POINT ( 'NONE',  ( -82.39999999999999147, -31.46250000000000568, 96.53589838486223584 ) ) ;
#14656 = CARTESIAN_POINT ( 'NONE',  ( 232.3466685930879123, -34.99995246259152282, -52.98928446312130802 ) ) ;
#14657 =( NAMED_UNIT ( * ) PLANE_ANGLE_UNIT ( ) SI_UNIT ( $, .RADIAN. ) );
#14658 = ADVANCED_FACE ( 'NONE', ( #4002 ), #10059, .F. ) ;
#14659 = CARTESIAN_POINT ( 'NONE',  ( 82.17437583783167554, -34.99999999999999289, 102.9802575795477679 ) ) ;
#14660 = CARTESIAN_POINT ( 'NONE',  ( -83.77821517812500929, -34.71562499938548285, 97.61286128772489690 ) ) ;
#14661 = CARTESIAN_POINT ( 'NONE',  ( 229.8435696437499871, -30.62812499938547717, 98.40857419181659793 ) ) ;
#14662 = ORIENTED_EDGE ( 'NONE', *, *, #18365, .F. ) ;
#14663 = CARTESIAN_POINT ( 'NONE',  ( -85.15643035624999868, -30.17812499938548498, -101.5914258081833879 ) ) ;
#14664 = DIRECTION ( 'NONE',  ( 0.000000000000000000, 0.000000000000000000, -1.000000000000000000 ) ) ;
#14665 =( BOUNDED_CURVE ( )  B_SPLINE_CURVE ( 2, ( #13052, #17457, #19018, #16081, #13137, #857, #19111, #6819, #5731 ),
 .UNSPECIFIED., .F., .F. ) 
 B_SPLINE_CURVE_WITH_KNOTS ( ( 3, 2, 2, 2, 3 ),
 ( 0.8125000000000000000, 0.8194444444444444198, 0.8333333333333333703, 0.8472222222222222099, 0.8541666666666665186 ),
 .UNSPECIFIED. ) 
 CURVE ( )  GEOMETRIC_REPRESENTATION_ITEM ( )  RATIONAL_B_SPLINE_CURVE ( ( 0.9330127018922194093, 0.9330127018922194093, 1.000000000000000000, 0.8660254037844387076, 1.000000000000000000, 0.8660254037844387076, 1.000000000000000000, 0.9330127018922209636, 0.9330127018922194093 ) ) 
 REPRESENTATION_ITEM ( '' )  );
#14666 = CARTESIAN_POINT ( 'NONE',  ( -79.39999999999999147, -33.31874999877096855, 99.99999999999998579 ) ) ;
#14667 = CARTESIAN_POINT ( 'NONE',  ( 232.5999999999999943, -34.86562499938548143, 96.81714838363319586 ) ) ;
#14668 = CARTESIAN_POINT ( 'NONE',  ( -85.15643035625001289, -35.20312499938548711, 99.99999999999998579 ) ) ;
#14669 = DIRECTION ( 'NONE',  ( -0.000000000000000000, -1.000000000000000000, -0.000000000000000000 ) ) ;
#14670 = CARTESIAN_POINT ( 'NONE',  ( 229.8435696437499303, -33.74062499938548143, -50.00000000000011369 ) ) ;
#14671 = ORIENTED_EDGE ( 'NONE', *, *, #2844, .T. ) ;
#14672 = VERTEX_POINT ( 'NONE', #14635 ) ;
#14673 = CARTESIAN_POINT ( 'NONE',  ( -84.41281071784420931, -32.00000000000000000, 98.10821574224533492 ) ) ;
#14674 = CARTESIAN_POINT ( 'NONE',  ( -81.02178482187500208, -34.94062499938548427, 102.3871387122750889 ) ) ;
#14675 = CARTESIAN_POINT ( 'NONE',  ( -94.79999999999999716, -35.00000000000000000, 150.0000000000000000 ) ) ;
#14676 = CARTESIAN_POINT ( 'NONE',  ( 85.15643035624999868, -34.60312499938548569, 98.40857419181659793 ) ) ;
#14677 = CARTESIAN_POINT ( 'NONE',  ( 85.40000000000000568, -34.08749999999999858, -98.26794919243111792 ) ) ;
#14678 = CARTESIAN_POINT ( 'NONE',  ( 229.8435696437499871, -30.62812499938547717, 98.40857419181659793 ) ) ;
#14679 = CARTESIAN_POINT ( 'NONE',  ( 232.5999999999999943, -33.85312499938547859, -53.18285161636690361 ) ) ;
#14680 = B_SPLINE_CURVE_WITH_KNOTS ( 'NONE', 3,
 ( #15478, #1281, #8698, #5424, #11364, #7229, #17233, #11266, #9805, #14098, #15672, #737, #13185, #2375, #12739, #8146 ),
 .UNSPECIFIED., .F., .F.,
 ( 4, 2, 2, 2, 2, 2, 2, 4 ),
 ( 0.000000000000000000, 0.0005391024520904662623, 0.001078204904180932525, 0.002156409808361806069, 0.002695512260452271030, 0.003234614712542735991, 0.003773717164633200519, 0.004312819616723665046 ),
 .UNSPECIFIED. ) ;
#14681 = CARTESIAN_POINT ( 'NONE',  ( -81.59615242270662350, -30.58259618943234059, 96.99999999999998579 ) ) ;
#14682 = CARTESIAN_POINT ( 'NONE',  ( 85.15643035624999868, -33.77812499938548285, 101.5914258081833879 ) ) ;
#14683 = CARTESIAN_POINT ( 'NONE',  ( 85.15643035625001289, -31.94062499938548427, -99.99999999999998579 ) ) ;
#14684 = CARTESIAN_POINT ( 'NONE',  ( 232.5999999999999375, -30.56250000000000000, -53.46410161513786363 ) ) ;
#14685 = CARTESIAN_POINT ( 'NONE',  ( -85.40000000000000568, -34.05000000000000426, 99.99999999999998579 ) ) ;
#14686 = CARTESIAN_POINT ( 'NONE',  ( 4.052416734886620908, -1.393505408945139301, -3.567979131523610459 ) ) ;
#14687 = ORIENTED_EDGE ( 'NONE', *, *, #7074, .T. ) ;
#14688 = LINE ( 'NONE', #17346, #15996 ) ;
#14689 = CARTESIAN_POINT ( 'NONE',  ( -83.90000000000000568, -34.96874999877096712, 97.40192378864668399 ) ) ;
#14690 = CARTESIAN_POINT ( 'NONE',  ( 235.3564303562499447, -31.86562499938547788, -48.40857419181671162 ) ) ;
#14691 = CARTESIAN_POINT ( 'NONE',  ( -83.77821517812500929, -32.91562499938547859, 97.61286128772489690 ) ) ;
#14692 = ORIENTED_EDGE ( 'NONE', *, *, #516, .T. ) ;
#14693 = CARTESIAN_POINT ( 'NONE',  ( -83.43443729601585801, -35.00000000000000000, 102.5775038898421201 ) ) ;
#14694 = CARTESIAN_POINT ( 'NONE',  ( 105.1999999999999886, -32.00000000000000711, -97.80000000000002558 ) ) ;
#14695 = PLANE ( 'NONE',  #18596 ) ;
#14696 = CARTESIAN_POINT ( 'NONE',  ( -79.39999999999999147, -32.50856250001229597, 101.7320508075688537 ) ) ;
#14697 =( BOUNDED_CURVE ( )  B_SPLINE_CURVE ( 2, ( #10407, #7283, #11968, #13526, #17936 ),
 .UNSPECIFIED., .F., .T. ) 
 B_SPLINE_CURVE_WITH_KNOTS ( ( 3, 2, 3 ),
 ( 0.2975293541897522931, 0.3055555555555555802, 0.3125000000000001665 ),
 .UNSPECIFIED. ) 
 CURVE ( )  GEOMETRIC_REPRESENTATION_ITEM ( )  RATIONAL_B_SPLINE_CURVE ( ( 0.9346381638529801528, 0.9225778897267638001, 1.000000000000000000, 0.9330127018922177440, 0.9330127018922194093 ) ) 
 REPRESENTATION_ITEM ( '' )  );
#14698 = CARTESIAN_POINT ( 'NONE',  ( -99.99999999999998579, -35.00000000000000000, 150.0000000000000000 ) ) ;
#14699 = CARTESIAN_POINT ( 'NONE',  ( 230.5523683116323355, -32.00000000000000000, -48.15470523285603832 ) ) ;
#14700 = CARTESIAN_POINT ( 'NONE',  ( -85.15643035624999868, -31.90312499938548285, 101.5914258081833879 ) ) ;
#14701 = PLANE ( 'NONE',  #525 ) ;
#14702 = CARTESIAN_POINT ( 'NONE',  ( 82.39999999999999147, -33.29062499938549280, 96.81714838363319586 ) ) ;
#14703 = DIRECTION ( 'NONE',  ( 1.000000000000000000, -0.000000000000000000, -2.407412430484046130E-31 ) ) ;
#14704 = CARTESIAN_POINT ( 'NONE',  ( -79.39999999999999147, -32.43750000000000000, -101.7320508075688963 ) ) ;
#14705 = CARTESIAN_POINT ( 'NONE',  ( 82.39999999999999147, -33.29062499938549280, -103.1828516163667899 ) ) ;
#14706 = CARTESIAN_POINT ( 'NONE',  ( -85.15643035625001289, -30.25312499938548783, -99.99999999999998579 ) ) ;
#14707 = ORIENTED_EDGE ( 'NONE', *, *, #16190, .F. ) ;
#14708 = CARTESIAN_POINT ( 'NONE',  ( 85.40000000000000568, -33.05624999877096570, 98.26794919243111792 ) ) ;
#14709 = DIRECTION ( 'NONE',  ( -1.000000000000000000, 0.000000000000000000, 0.000000000000000000 ) ) ;
#14710 = DIRECTION ( 'NONE',  ( -0.000000000000000000, 0.000000000000000000, -1.000000000000000000 ) ) ;
#14711 = VECTOR ( 'NONE', #12762, 1000.000000000000000 ) ;
#14712 = VECTOR ( 'NONE', #15040, 1000.000000000000000 ) ;
#14713 = CARTESIAN_POINT ( 'NONE',  ( -82.39999999999999147, -30.36562499938549209, 96.81714838363319586 ) ) ;
#14714 = CARTESIAN_POINT ( 'NONE',  ( 81.22643902601967625, -31.99999999999998579, 102.6636594982983155 ) ) ;
#14715 = EDGE_LOOP ( 'NONE', ( #9655, #15231, #8065, #14161 ) ) ;
#14716 = CARTESIAN_POINT ( 'NONE',  ( -79.64356964374999848, -33.51562499938548711, -99.99999999999998579 ) ) ;
#14717 = CARTESIAN_POINT ( 'NONE',  ( 0.3126073911695752550, -2.020725942163798194, -3.500000000000000000 ) ) ;
#14718 = EDGE_CURVE ( 'NONE', #5869, #13533, #10153, .T. ) ;
#14719 = ORIENTED_EDGE ( 'NONE', *, *, #4946, .F. ) ;
#14720 = CARTESIAN_POINT ( 'NONE',  ( 85.15643035625001289, -34.79062499938548569, 101.5914258081833879 ) ) ;
#14721 = CARTESIAN_POINT ( 'NONE',  ( -81.02178482187500208, -34.45312499938548711, -102.3871387122750889 ) ) ;
#14722 = DIRECTION ( 'NONE',  ( 0.000000000000000000, -0.000000000000000000, -1.000000000000000000 ) ) ;
#14723 = CARTESIAN_POINT ( 'NONE',  ( -85.40000000000000568, -31.70624999877096784, -98.26794919243111792 ) ) ;
#14724 = CARTESIAN_POINT ( 'NONE',  ( 229.8435696437499871, -30.74062499938547433, 98.40857419181659793 ) ) ;
#14725 = CARTESIAN_POINT ( 'NONE',  ( -80.90000000000000568, -34.29374999877096997, 102.5980762113533018 ) ) ;
#14726 = CARTESIAN_POINT ( 'NONE',  ( -85.15643035624999868, -32.91562499938549280, 101.5914258081833879 ) ) ;
#14727 = CARTESIAN_POINT ( 'NONE',  ( -85.15643035625001289, -34.19062499938548427, -99.99999999999998579 ) ) ;
#14728 = FACE_OUTER_BOUND ( 'NONE', #771, .T. ) ;
#14729 = VECTOR ( 'NONE', #13116, 1000.000000000000000 ) ;
#14730 = CARTESIAN_POINT ( 'NONE',  ( 234.9210568921013191, -34.99999999999998579, 101.4973817956047668 ) ) ;
#14731 = EDGE_CURVE ( 'NONE', #18235, #2812, #15921, .T. ) ;
#14732 = CARTESIAN_POINT ( 'NONE',  ( 80.90000000000000568, -31.89374999877096784, -97.40192378864668399 ) ) ;
#14733 = CARTESIAN_POINT ( 'NONE',  ( 231.0999999999999375, -33.52499999999999147, 102.5980762113533018 ) ) ;
#14734 = EDGE_CURVE ( 'NONE', #16323, #13062, #9864, .T. ) ;
#14735 = ORIENTED_EDGE ( 'NONE', *, *, #4601, .F. ) ;
#14736 = CARTESIAN_POINT ( 'NONE',  ( 82.39999999999999147, -34.30312499938548143, -96.81714838363319586 ) ) ;
#14737 = CARTESIAN_POINT ( 'NONE',  ( 235.5999999999999943, -33.80624999877096570, 101.7320508075688537 ) ) ;
#14738 = CARTESIAN_POINT ( 'NONE',  ( 231.0999999999999375, -32.56874999877096144, -47.40192378864679768 ) ) ;
#14739 = ADVANCED_FACE ( 'NONE', ( #19142 ), #2524, .F. ) ;
#14740 = CARTESIAN_POINT ( 'NONE',  ( -79.64356964374998427, -32.65312499938548285, 101.5914258081833879 ) ) ;
#14741 = ORIENTED_EDGE ( 'NONE', *, *, #11980, .F. ) ;
#14742 = ORIENTED_EDGE ( 'NONE', *, *, #1479, .T. ) ;
#14743 = CARTESIAN_POINT ( 'NONE',  ( -84.11496519894868129, -32.00000000000000000, 97.81539907810714851 ) ) ;
#14744 = CIRCLE ( 'NONE', #12882, 0.5155456020628804703 ) ;
#14745 = CARTESIAN_POINT ( 'NONE',  ( -82.39999999999999147, -34.33124999877097139, 103.0000000000000000 ) ) ;
#14746 = CIRCLE ( 'NONE', #12257, 3.000000000000002665 ) ;
#14747 = CARTESIAN_POINT ( 'NONE',  ( 111.5000000000000142, 12.69999999999998508, 110.0000000000000142 ) ) ;
#14748 = ORIENTED_EDGE ( 'NONE', *, *, #11514, .T. ) ;
#14749 = CARTESIAN_POINT ( 'NONE',  ( -81.79008970393687150, -34.99999999999997868, 102.6939647107541873 ) ) ;
#14750 = CARTESIAN_POINT ( 'NONE',  ( 82.40000000000000568, -30.00000000000000355, 99.99999999999998579 ) ) ;
#14751 = CARTESIAN_POINT ( 'NONE',  ( 5.599999999999999645, -4.041451884327388555, 0.000000000000000000 ) ) ;
#14752 = CARTESIAN_POINT ( 'NONE',  ( -85.15643035624999868, -35.16562499938547859, 101.5914258081833879 ) ) ;
#14753 = CARTESIAN_POINT ( 'NONE',  ( -80.90000000000000568, -33.00000000000000000, 102.5980762113533018 ) ) ;
#14754 = EDGE_CURVE ( 'NONE', #5593, #15949, #4620, .T. ) ;
#14755 = CARTESIAN_POINT ( 'NONE',  ( -82.39999999999999147, -30.95624999877097139, 96.53589838486223584 ) ) ;
#14756 = CARTESIAN_POINT ( 'NONE',  ( -82.40000000000000568, -30.33749999999999858, 102.9999999999999858 ) ) ;
#14757 = DIRECTION ( 'NONE',  ( 0.000000000000000000, 0.000000000000000000, -1.000000000000000000 ) ) ;
#14758 = CARTESIAN_POINT ( 'NONE',  ( -82.39999999999999147, -34.75312499938549138, 96.81714838363319586 ) ) ;
#14759 = VECTOR ( 'NONE', #17310, 1000.000000000000000 ) ;
#14760 =( BOUNDED_CURVE ( )  B_SPLINE_CURVE ( 2, ( #1332, #10314, #18921, #2494, #7278, #14500, #19207, #8452, #11582, #7185, #5822, #1231, #1132, #11677, #17748, #17643, #4351, #18827, #14405, #2883, #1044, #16271, #8839, #7375, #5450, #6996, #17547, #12949, #8548, #10215, #2587, #16077, #7091, #17353, #19108, #10121, #13048, #3963, #13134, #19016, #5542, #5728, #4163, #17453, #4066, #8642, #14602, #10690, #12160, #14996, #3072, #7764, #4543, #4743, #14894, #13717, #4842, #19309, #7474, #7568, #3165, #1705, #15281, #358, #5920, #6213, #1896, #10598, #3361, #4649, #10403, #13522, #9217, #10785, #13431, #16367, #3259, #9032, #16657, #2975, #159, #16562, #8931 ),
 .UNSPECIFIED., .F., .F. ) 
 B_SPLINE_CURVE_WITH_KNOTS ( ( 3, 2, 2, 2, 2, 2, 2, 2, 2, 2, 2, 2, 2, 2, 2, 2, 2, 2, 2, 2, 2, 2, 2, 2, 2, 2, 2, 2, 2, 2, 2, 2, 2, 2, 2, 2, 2, 2, 2, 2, 2, 3 ),
 ( 0.3716916592826012278, 0.3750191855951753306, 0.3900199530189823460, 0.4050207204427893615, 0.4200214878665964324, 0.4350222552904034479, 0.4500230227142104633, 0.4650237901380174788, 0.4800245575618244387, 0.4950253249856314541, 0.5100260924094385251, 0.5250268598332454850, 0.5400276272570525560, 0.5550283946808595159, 0.5700291621046665869, 0.5850299295284735468, 0.6000306969522806178, 0.6150314643760875777, 0.6300322317998946486, 0.6450329992237016086, 0.6600337666475086795, 0.6750345340713157505, 0.6900353014951225994, 0.7050360689189296703, 0.7200368363427367413, 0.7350376037665438123, 0.7500383711903507722, 0.7650391386141577321, 0.7800399060379648031, 0.7950406734617718740, 0.8100414408855788340, 0.8250422083093857939, 0.8400429757331928649, 0.8550437431569999358, 0.8700445105808070068, 0.8850452780046138557, 0.9000460454284209266, 0.9150468128522277755, 0.9300475802760350685, 0.9450483476998419174, 0.9600491151236489884, 0.9717223562348840105 ),
 .UNSPECIFIED. ) 
 CURVE ( )  GEOMETRIC_REPRESENTATION_ITEM ( )  RATIONAL_B_SPLINE_CURVE ( ( 0.9537471549767004841, 0.9702812541832854798, 1.000000000000000000, 0.8660254037844387076, 1.000000000000000000, 0.8660254037844387076, 1.000000000000000000, 0.8660254037844387076, 1.000000000000000000, 0.8660254037844387076, 1.000000000000000000, 0.8660254037844387076, 1.000000000000000000, 0.8660254037844387076, 1.000000000000000000, 0.8660254037844387076, 1.000000000000000000, 0.8660254037844387076, 1.000000000000000000, 0.8660254037844387076, 1.000000000000000000, 0.8660254037844387076, 1.000000000000000000, 0.8660254037844387076, 1.000000000000000000, 0.8660254037844387076, 1.000000000000000000, 0.8660254037844387076, 1.000000000000000000, 0.8660254037844387076, 1.000000000000000000, 0.8660254037844387076, 1.000000000000000000, 0.8660254037844387076, 1.000000000000000000, 0.8660254037844387076, 1.000000000000000000, 0.8660254037844387076, 1.000000000000000000, 0.8660254037844387076, 1.000000000000000000, 0.8660254037844387076, 1.000000000000000000, 0.8660254037844387076, 1.000000000000000000, 0.8660254037844387076, 1.000000000000000000, 0.8660254037844387076, 1.000000000000000000, 0.8660254037844387076, 1.000000000000000000, 0.8660254037844387076, 1.000000000000000000, 0.8660254037844387076, 1.000000000000000000, 0.8660254037844387076, 1.000000000000000000, 0.8660254037844387076, 1.000000000000000000, 0.8660254037844387076, 1.000000000000000000, 0.8660254037844387076, 1.000000000000000000, 0.8660254037844387076, 1.000000000000000000, 0.8660254037844387076, 1.000000000000000000, 0.8660254037844387076, 1.000000000000000000, 0.8660254037844387076, 1.000000000000000000, 0.8660254037844387076, 1.000000000000000000, 0.8660254037844387076, 1.000000000000000000, 0.8660254037844387076, 1.000000000000000000, 0.8660254037844387076, 1.000000000000000000, 0.8660254037844387076, 1.000000000000000000, 0.8957441496011343540, 0.9537471549767215784 ) ) 
 REPRESENTATION_ITEM ( '' )  );
#14761 = CARTESIAN_POINT ( 'NONE',  ( 233.9782151781249411, -30.44062499938548072, 102.3871387122750889 ) ) ;
#14762 = VERTEX_POINT ( 'NONE', #11524 ) ;
#14763 = CARTESIAN_POINT ( 'NONE',  ( -85.15643035624999868, -35.22676555956768141, -101.0032586025029815 ) ) ;
#14764 = CARTESIAN_POINT ( 'NONE',  ( -82.40000000000000568, -33.71249999999998437, 96.99999999999998579 ) ) ;
#14765 = CARTESIAN_POINT ( 'NONE',  ( 232.5999999999999375, -33.93749999999999289, 103.0000000000000000 ) ) ;
#14766 = DIRECTION ( 'NONE',  ( -1.000000000000000000, -0.000000000000000000, -0.000000000000000000 ) ) ;
#14767 = CARTESIAN_POINT ( 'NONE',  ( -81.02178482187500208, -30.89062499938548711, 102.3871387122750889 ) ) ;
#14768 = PLANE ( 'NONE',  #5068 ) ;
#14769 = EDGE_CURVE ( 'NONE', #14513, #10474, #9455, .T. ) ;
#14770 = CARTESIAN_POINT ( 'NONE',  ( 229.8435696437499303, -33.29062499938547148, -50.00000000000011369 ) ) ;
#14771 = ORIENTED_EDGE ( 'NONE', *, *, #8320, .T. ) ;
#14772 = EDGE_LOOP ( 'NONE', ( #17345, #5868, #10310, #476 ) ) ;
#14773 = CARTESIAN_POINT ( 'NONE',  ( -84.69814068649969840, -35.00052333152936512, -101.9283540611242955 ) ) ;
#14774 = CARTESIAN_POINT ( 'NONE',  ( -85.40000000000000568, -32.28750000000000142, 98.26794919243111792 ) ) ;
#14775 = CARTESIAN_POINT ( 'NONE',  ( -83.90000000000000568, -32.11874999877097281, 102.5980762113533018 ) ) ;
#14776 = CARTESIAN_POINT ( 'NONE',  ( 83.90000000000000568, -30.07499999999999929, 102.5980762113533018 ) ) ;
#14777 = EDGE_CURVE ( 'NONE', #1022, #15818, #15388, .T. ) ;
#14778 = PRODUCT_DEFINITION ( 'UNKNOWN', '', #10502, #13727 ) ;
#14779 = CARTESIAN_POINT ( 'NONE',  ( -85.40000000000000568, -32.70000000000000284, 99.99999999999998579 ) ) ;
#14780 = CARTESIAN_POINT ( 'NONE',  ( 231.2217848218749339, -32.31562499938547717, 102.3871387122750889 ) ) ;
#14781 = CARTESIAN_POINT ( 'NONE',  ( 231.2217848218749339, -34.26562499938548001, -52.38713871227520968 ) ) ;
#14782 = CARTESIAN_POINT ( 'NONE',  ( 85.15643035624999868, -34.60312499938548569, 98.40857419181659793 ) ) ;
#14783 =( BOUNDED_CURVE ( )  B_SPLINE_CURVE ( 2, ( #9444, #14222, #576, #18350, #14037, #5155, #12383, #11101, #8180 ),
 .UNSPECIFIED., .F., .F. ) 
 B_SPLINE_CURVE_WITH_KNOTS ( ( 3, 2, 2, 2, 3 ),
 ( 0.5625000000000000000, 0.5694444444444444198, 0.5833333333333333703, 0.5972222222222222099, 0.6041666666666666297 ),
 .UNSPECIFIED. ) 
 CURVE ( )  GEOMETRIC_REPRESENTATION_ITEM ( )  RATIONAL_B_SPLINE_CURVE ( ( 0.9330127018922194093, 0.9330127018922194093, 1.000000000000000000, 0.8660254037844387076, 1.000000000000000000, 0.8660254037844387076, 1.000000000000000000, 0.9330127018922198534, 0.9330127018922192983 ) ) 
 REPRESENTATION_ITEM ( '' )  );
#14784 = CARTESIAN_POINT ( 'NONE',  ( 79.64356964375001269, -32.12812499938548427, -98.40857419181659793 ) ) ;
#14785 = CARTESIAN_POINT ( 'NONE',  ( 234.0999999999999375, -30.14999999999999503, -52.59807621135342970 ) ) ;
#14786 = CARTESIAN_POINT ( 'NONE',  ( -79.39999999999999147, -31.51874999877096784, 99.99999999999998579 ) ) ;
#14787 = CARTESIAN_POINT ( 'NONE',  ( 85.15643035625001289, -32.84062499938548285, -99.99999999999998579 ) ) ;
#14788 = ORIENTED_EDGE ( 'NONE', *, *, #4540, .F. ) ;
#14789 = CARTESIAN_POINT ( 'NONE',  ( 0.000000000000000000, 3.031088913245533867, 1.750000000000002887 ) ) ;
#14790 = CYLINDRICAL_SURFACE ( 'NONE', #11791, 3.000000000000002665 ) ;
#14791 = CARTESIAN_POINT ( 'NONE',  ( 232.5999999999999375, -31.04062499938547859, -46.81714838363331666 ) ) ;
#14792 = CARTESIAN_POINT ( 'NONE',  ( -79.64356964375001269, -32.20312499938548001, 101.5914258081833879 ) ) ;
#14793 = EDGE_LOOP ( 'NONE', ( #13380, #13246, #10632, #11905, #16715, #14707, #7628, #4708, #1082, #9459, #12205, #7924, #7296, #18200, #243, #12108, #3864 ) ) ;
#14794 = CARTESIAN_POINT ( 'NONE',  ( -82.40000000000001990, -33.88124999877096855, 103.0000000000000000 ) ) ;
#14795 = CARTESIAN_POINT ( 'NONE',  ( 3.973110223767137850, -2.261515145575163828E-11, -3.565797985667433778 ) ) ;
#14796 = CARTESIAN_POINT ( 'NONE',  ( 81.05805657947855991, -34.99999999999999289, -97.38506107425206437 ) ) ;
#14797 = CARTESIAN_POINT ( 'NONE',  ( -82.39999999999999147, -31.45856250001229881, 96.53589838486223584 ) ) ;
#14798 = DIRECTION ( 'NONE',  ( -1.000000000000000000, -0.000000000000000000, -0.000000000000000000 ) ) ;
#14799 = CARTESIAN_POINT ( 'NONE',  ( 84.70388354820684640, -35.00002705695777649, -98.07851859032987818 ) ) ;
#14800 = CARTESIAN_POINT ( 'NONE',  ( -81.02178482187500208, -31.64062499938548356, 97.61286128772489690 ) ) ;
#14801 = CARTESIAN_POINT ( 'NONE',  ( 84.97866794691726966, -32.00000000000000000, 100.9899807706011927 ) ) ;
#14802 = CARTESIAN_POINT ( 'NONE',  ( 82.39999999999999147, -31.71562499938548640, 103.1828516163667899 ) ) ;
#14803 = FACE_OUTER_BOUND ( 'NONE', #10719, .T. ) ;
#14804 = CARTESIAN_POINT ( 'NONE',  ( 231.0999999999999375, -33.07499999999999574, -47.40192378864679768 ) ) ;
#14805 = CARTESIAN_POINT ( 'NONE',  ( -79.64356964374999848, -32.72812499938548569, 99.99999999999998579 ) ) ;
#14806 = CARTESIAN_POINT ( 'NONE',  ( -85.15643035624999868, -31.11562499938548854, -98.40857419181659793 ) ) ;
#14807 = EDGE_LOOP ( 'NONE', ( #16312, #17826, #10463 ) ) ;
#14808 = CARTESIAN_POINT ( 'NONE',  ( 83.90000000000000568, -34.06874999877096855, 102.5980762113533018 ) ) ;
#14809 = CARTESIAN_POINT ( 'NONE',  ( -82.40000000000000568, -34.78124999877096712, 102.9999999999999858 ) ) ;
#14810 = CARTESIAN_POINT ( 'NONE',  ( 231.2217848218749339, -34.82812499938548001, -52.38713871227520968 ) ) ;
#14811 = CARTESIAN_POINT ( 'NONE',  ( -83.77821517812500929, -31.22812499938548569, 97.61286128772489690 ) ) ;
#14812 = CARTESIAN_POINT ( 'NONE',  ( 79.79868554281867432, -31.99999999999999289, 101.4716133421946012 ) ) ;
#14813 = ORIENTED_EDGE ( 'NONE', *, *, #1001, .T. ) ;
#14814 = CARTESIAN_POINT ( 'NONE',  ( -82.39999999999999147, -34.52812499938548996, -96.81714838363319586 ) ) ;
#14815 =( BOUNDED_CURVE ( )  B_SPLINE_CURVE ( 2, ( #6353, #6548, #10934, #16804, #12306, #16610, #3217, #16516, #12493 ),
 .UNSPECIFIED., .F., .F. ) 
 B_SPLINE_CURVE_WITH_KNOTS ( ( 3, 2, 2, 2, 3 ),
 ( 0.1458333333333334814, 0.1527777777777777901, 0.1666666666666666574, 0.1805555555555555525, 0.1875000000000000278 ),
 .UNSPECIFIED. ) 
 CURVE ( )  GEOMETRIC_REPRESENTATION_ITEM ( )  RATIONAL_B_SPLINE_CURVE ( ( 0.9330127018922194093, 0.9330127018922207416, 1.000000000000000000, 0.8660254037844387076, 1.000000000000000000, 0.8660254037844387076, 1.000000000000000000, 0.9330127018922190762, 0.9330127018922194093 ) ) 
 REPRESENTATION_ITEM ( '' )  );
#14816 = LINE ( 'NONE', #16490, #1929 ) ;
#14817 = CARTESIAN_POINT ( 'NONE',  ( 232.5999999999999375, -33.71249999999999147, -53.00000000000010658 ) ) ;
#14818 = CARTESIAN_POINT ( 'NONE',  ( -79.64356964375001269, -32.76562499938548711, -98.40857419181659793 ) ) ;
#14819 = DIRECTION ( 'NONE',  ( -0.000000000000000000, -1.000000000000000000, 3.597944987211154374E-15 ) ) ;
#14820 = CARTESIAN_POINT ( 'NONE',  ( -85.40000000000000568, -30.80624999877096926, -98.26794919243111792 ) ) ;
#14821 = CARTESIAN_POINT ( 'NONE',  ( 229.8435696437499871, -32.99062499938548143, 98.40857419181659793 ) ) ;
#14822 = CARTESIAN_POINT ( 'NONE',  ( -83.90000000000000568, -31.37268749875867613, 97.40192378864668399 ) ) ;
#14823 = B_SPLINE_CURVE_WITH_KNOTS ( 'NONE', 3,
 ( #7935, #12620, #2359, #16837, #15753, #9695 ),
 .UNSPECIFIED., .F., .F.,
 ( 4, 2, 4 ),
 ( 0.01103795673506154963, 0.01206113197427181698, 0.01308430721348208606 ),
 .UNSPECIFIED. ) ;
#14824 = CARTESIAN_POINT ( 'NONE',  ( -82.39999999999999147, -33.29062499938549280, 103.1828516163667899 ) ) ;
#14825 = CARTESIAN_POINT ( 'NONE',  ( -83.77821517812500929, -34.11562499938548854, -97.61286128772489690 ) ) ;
#14826 = DIRECTION ( 'NONE',  ( -1.000000000000000000, 0.000000000000000000, 0.000000000000000000 ) ) ;
#14827 = CIRCLE ( 'NONE', #5787, 6.000000000000015987 ) ;
#14828 = CARTESIAN_POINT ( 'NONE',  ( -82.40000000000000568, -30.00000000000000355, -99.99999999999998579 ) ) ;
#14829 = CARTESIAN_POINT ( 'NONE',  ( 80.90000000000000568, -34.59374999877096712, -97.40192378864668399 ) ) ;
#14830 = CARTESIAN_POINT ( 'NONE',  ( 231.0999999999999375, -32.77499999999999147, 97.40192378864668399 ) ) ;
#14831 = EDGE_CURVE ( 'NONE', #1510, #14649, #8717, .T. ) ;
#14832 = EDGE_CURVE ( 'NONE', #9677, #11976, #2605, .T. ) ;
#14833 = ORIENTED_EDGE ( 'NONE', *, *, #5799, .F. ) ;
#14834 = CARTESIAN_POINT ( 'NONE',  ( 79.64356964374998427, -34.82812499938548711, -98.40857419181659793 ) ) ;
#14835 = CARTESIAN_POINT ( 'NONE',  ( 231.2217848218749339, -30.77812499938548285, 97.61286128772489690 ) ) ;
#14836 = CARTESIAN_POINT ( 'NONE',  ( 235.5999999999999375, -34.66874999877096286, -50.00000000000011369 ) ) ;
#14837 = CARTESIAN_POINT ( 'NONE',  ( -85.15643035625001289, -33.70312499938548711, 101.5914258081833879 ) ) ;
#14838 = ORIENTED_EDGE ( 'NONE', *, *, #8397, .T. ) ;
#14839 = ORIENTED_EDGE ( 'NONE', *, *, #8801, .F. ) ;
#14840 = CARTESIAN_POINT ( 'NONE',  ( 80.90000000000000568, -34.35000000000000853, -102.5980762113533018 ) ) ;
#14841 = VECTOR ( 'NONE', #14899, 1000.000000000000000 ) ;
#14842 = FACE_OUTER_BOUND ( 'NONE', #15213, .T. ) ;
#14843 = CARTESIAN_POINT ( 'NONE',  ( 234.0999999999999375, -34.19999999999999574, -52.59807621135342970 ) ) ;
#14844 = ORIENTED_EDGE ( 'NONE', *, *, #15183, .F. ) ;
#14845 = CARTESIAN_POINT ( 'NONE',  ( -82.85452780460292388, -35.00000000000000711, 102.7245357809972433 ) ) ;
#14846 = FACE_OUTER_BOUND ( 'NONE', #18577, .T. ) ;
#14847 = EDGE_CURVE ( 'NONE', #6709, #3185, #5857, .T. ) ;
#14848 = CARTESIAN_POINT ( 'NONE',  ( -81.02178482187500208, -32.80312499938548854, 102.3871387122750889 ) ) ;
#14849 = CARTESIAN_POINT ( 'NONE',  ( -85.40000000000000568, -34.95000000000000284, 99.99999999999998579 ) ) ;
#14850 = ADVANCED_FACE ( 'NONE', ( #1366 ), #9063, .F. ) ;
#14851 = CARTESIAN_POINT ( 'NONE',  ( -85.40000000000000568, -30.43124999877096926, 98.26794919243111792 ) ) ;
#14852 = CARTESIAN_POINT ( 'NONE',  ( 1.567478505476134606E-15, 4.618802153517012066, -5.000000000000000000 ) ) ;
#14853 = STYLED_ITEM ( 'NONE', ( #8690 ), #9020 ) ;
#14854 = CARTESIAN_POINT ( 'NONE',  ( -3.333333333333332149, -2.694301256218264218, -3.300726591567082036 ) ) ;
#14855 = FACE_OUTER_BOUND ( 'NONE', #3613, .T. ) ;
#14856 = VECTOR ( 'NONE', #16517, 1000.000000000000000 ) ;
#14857 = DIRECTION ( 'NONE',  ( -0.000000000000000000, -0.000000000000000000, 1.000000000000000000 ) ) ;
#14858 = VERTEX_POINT ( 'NONE', #7311 ) ;
#14859 =( LENGTH_UNIT ( ) NAMED_UNIT ( * ) SI_UNIT ( .MILLI., .METRE. ) );
#14860 = CARTESIAN_POINT ( 'NONE',  ( -82.39999999999999147, -34.07812499938548711, -96.81714838363319586 ) ) ;
#14861 = CARTESIAN_POINT ( 'NONE',  ( 235.5999999999999375, -32.47499999999999432, -50.00000000000011369 ) ) ;
#14862 = PLANE ( 'NONE',  #17072 ) ;
#14863 = DIRECTION ( 'NONE',  ( -1.000000000000000000, 4.625929269271485791E-17, -5.836151346627967635E-31 ) ) ;
#14864 = CARTESIAN_POINT ( 'NONE',  ( -83.77821517812500929, -31.86562499938548498, 102.3871387122750889 ) ) ;
#14865 = CARTESIAN_POINT ( 'NONE',  ( -85.40000000000000568, -34.05000000000000426, 99.99999999999998579 ) ) ;
#14866 = CARTESIAN_POINT ( 'NONE',  ( 229.8435696437499871, -33.25312499938547717, -48.40857419181671162 ) ) ;
#14867 = DIRECTION ( 'NONE',  ( -0.000000000000000000, -1.000000000000000000, -0.000000000000000000 ) ) ;
#14868 = VERTEX_POINT ( 'NONE', #13652 ) ;
#14869 = ORIENTED_EDGE ( 'NONE', *, *, #17616, .F. ) ;
#14870 = CARTESIAN_POINT ( 'NONE',  ( -84.97866794691721282, -31.99999999999999289, 99.01001922939857991 ) ) ;
#14871 = CARTESIAN_POINT ( 'NONE',  ( -83.90000000000000568, -31.72500000000000142, 102.5980762113533018 ) ) ;
#14872 = CARTESIAN_POINT ( 'NONE',  ( -83.90000000000000568, -32.26874999877097139, 97.40192378864668399 ) ) ;
#14873 = CARTESIAN_POINT ( 'NONE',  ( 79.39999999999999147, -31.57499999999999929, 99.99999999999998579 ) ) ;
#14874 = CARTESIAN_POINT ( 'NONE',  ( 83.20384757729335945, -33.45134618820330985, 96.99999999999998579 ) ) ;
#14875 = CARTESIAN_POINT ( 'NONE',  ( 235.3564303562499447, -33.51562499938548001, 99.99999999999998579 ) ) ;
#14876 =( BOUNDED_SURFACE ( )  B_SPLINE_SURFACE ( 3, 2, ( 
 ( #14921, #10424, #19228 ),
 ( #11696, #17665, #4565 ),
 ( #13542, #1548, #10241 ),
 ( #2811, #6039, #16205 ),
 ( #1355, #13452, #17767 ),
 ( #183, #7298, #1442 ) ),
 .UNSPECIFIED., .F., .F., .F. ) 
 B_SPLINE_SURFACE_WITH_KNOTS ( ( 4, 2, 4 ),
 ( 3, 3 ),
 ( 0.02027065861071770947, 0.02273072267836921331, 0.02519078674602071716 ),
 ( 0.000000000000000000, 1.000000000000000000 ),
 .UNSPECIFIED. ) 
 GEOMETRIC_REPRESENTATION_ITEM ( )  RATIONAL_B_SPLINE_SURFACE ( (
 ( 1.000000000000000000, 0.8047781708337304885, 1.000000000000000000),
 ( 1.000000000000000000, 0.8123765190705307671, 1.000000000000000000),
 ( 1.000000000000000000, 0.8190656277163975707, 1.000000000000000000),
 ( 1.000000000000000000, 0.8192366903512159348, 1.000000000000000000),
 ( 1.000000000000000000, 0.8126138454302893610, 1.000000000000000000),
 ( 1.000000000000000000, 0.8047712246031417660, 1.000000000000000000) ) ) 
 REPRESENTATION_ITEM ( '' )  SURFACE ( )  );
#14877 = CARTESIAN_POINT ( 'NONE',  ( 233.9782151781249411, -33.59062499938547575, -47.61286128772501769 ) ) ;
#14878 = VECTOR ( 'NONE', #5982, 1000.000000000000000 ) ;
#14879 = CARTESIAN_POINT ( 'NONE',  ( 85.15643035625001289, -35.09062499938548285, 99.99999999999998579 ) ) ;
#14880 = CARTESIAN_POINT ( 'NONE',  ( 79.64356964375001269, -30.32812499938548711, -98.40857419181659793 ) ) ;
#14881 = ORIENTED_EDGE ( 'NONE', *, *, #16870, .F. ) ;
#14882 = CARTESIAN_POINT ( 'NONE',  ( 229.5999999999999375, -30.44999999999999574, -50.00000000000011369 ) ) ;
#14883 = LINE ( 'NONE', #13423, #1649 ) ;
#14884 = CARTESIAN_POINT ( 'NONE',  ( 82.39999999999999147, -32.95312499938548711, -96.81714838363319586 ) ) ;
#14885 = AXIS2_PLACEMENT_3D ( 'NONE', #15612, #578, #6532 ) ;
#14886 = VERTEX_POINT ( 'NONE', #4579 ) ;
#14887 = CYLINDRICAL_SURFACE ( 'NONE', #2882, 3.000000000000002665 ) ;
#14888 = ADVANCED_FACE ( 'NONE', ( #16309 ), #6144, .F. ) ;
#14889 = CARTESIAN_POINT ( 'NONE',  ( -84.01447415327271528, -35.02670941564510088, 97.25687757881057394 ) ) ;
#14890 = CARTESIAN_POINT ( 'NONE',  ( -79.39999999999999147, -31.16250000000000497, 101.7320508075688537 ) ) ;
#14891 = VERTEX_POINT ( 'NONE', #11811 ) ;
#14892 = CARTESIAN_POINT ( 'NONE',  ( -85.40000000000000568, -34.03124999877096712, 98.26794919243111792 ) ) ;
#14893 = AXIS2_PLACEMENT_3D ( 'NONE', #6032, #19124, #10418 ) ;
#14894 = CARTESIAN_POINT ( 'NONE',  ( 235.3564303562499447, -33.96562499938547575, 99.99999999999998579 ) ) ;
#14895 = CARTESIAN_POINT ( 'NONE',  ( 81.02178482187500208, -30.29062499938548569, 102.3871387122750889 ) ) ;
#14896 = CARTESIAN_POINT ( 'NONE',  ( -85.40000000000000568, -32.73356250001228318, 98.26794919243111792 ) ) ;
#14897 = AXIS2_PLACEMENT_3D ( 'NONE', #8326, #12624, #2549 ) ;
#14898 = COLOUR_RGB ( '',0.8941176470588234615, 0.8941176470588234615, 0.8941176470588234615 ) ;
#14899 = DIRECTION ( 'NONE',  ( 0.000000000000000000, -1.000000000000000000, 0.000000000000000000 ) ) ;
#14900 = B_SPLINE_CURVE_WITH_KNOTS ( 'NONE', 3,
 ( #14617, #12778, #3981, #9947, #869, #5741, #1248, #6834, #2509, #8466, #14423, #19123, #3883, #17659, #9847, #4271 ),
 .UNSPECIFIED., .F., .F.,
 ( 4, 2, 2, 2, 2, 2, 2, 4 ),
 ( 0.000000000000000000, 0.0005391024520903885250, 0.001078204904180777050, 0.002156409808361623923, 0.002695512260452052021, 0.003234614712542480553, 0.003773717164632909085, 0.004312819616723337184 ),
 .UNSPECIFIED. ) ;
#14901 = CARTESIAN_POINT ( 'NONE',  ( -85.40000000000000568, -32.21250000000000568, 101.7320508075688821 ) ) ;
#14902 = CARTESIAN_POINT ( 'NONE',  ( -79.64356964374999848, -31.71562499938548285, 99.99999999999998579 ) ) ;
#14903 = CARTESIAN_POINT ( 'NONE',  ( 229.8966310988167550, -35.00000000000000711, 100.9939266215705089 ) ) ;
#14904 = CARTESIAN_POINT ( 'NONE',  ( 82.39999999999999147, -33.06562499938548427, 103.1828516163667899 ) ) ;
#14905 = DIRECTION ( 'NONE',  ( 1.000000000000000000, 0.000000000000000000, -0.000000000000000000 ) ) ;
#14906 = CIRCLE ( 'NONE', #894, 2.649999999999980371 ) ;
#14907 = FACE_OUTER_BOUND ( 'NONE', #8571, .T. ) ;
#14908 = DIRECTION ( 'NONE',  ( -0.000000000000000000, -1.000000000000000000, -0.000000000000000000 ) ) ;
#14909 = CARTESIAN_POINT ( 'NONE',  ( -79.64356964375001269, -31.34062499938548640, -101.5914258081833879 ) ) ;
#14910 = EDGE_LOOP ( 'NONE', ( #2090, #8695, #14943, #5127 ) ) ;
#14911 = CARTESIAN_POINT ( 'NONE',  ( 82.39999999999999147, -31.26562499938549067, 103.1828516163667899 ) ) ;
#14912 = CARTESIAN_POINT ( 'NONE',  ( -94.79999999999999716, -29.80000000000000426, 150.0000000000000000 ) ) ;
#14913 = CARTESIAN_POINT ( 'NONE',  ( 229.8435696437499871, -34.71562499938548285, -48.40857419181671162 ) ) ;
#14914 = CIRCLE ( 'NONE', #7110, 2.100000000000000089 ) ;
#14915 = CARTESIAN_POINT ( 'NONE',  ( -83.90000000000000568, -33.07500000000000284, 102.5980762113533018 ) ) ;
#14916 = AXIS2_PLACEMENT_3D ( 'NONE', #11658, #4237, #12929 ) ;
#14917 = CARTESIAN_POINT ( 'NONE',  ( -82.39999999999999147, -31.71562499938548640, 96.81714838363319586 ) ) ;
#14918 = CARTESIAN_POINT ( 'NONE',  ( 81.59615242270665192, -33.86115380933864571, -103.0000000000000000 ) ) ;
#14919 = ORIENTED_EDGE ( 'NONE', *, *, #6263, .F. ) ;
#14920 = CARTESIAN_POINT ( 'NONE',  ( -82.39999999999999147, -30.33750000000000213, -96.53589838486223584 ) ) ;
#14921 = CARTESIAN_POINT ( 'NONE',  ( 4.000000000000000000, -2.511475576507276042, -3.469253905236643565 ) ) ;
#14922 = CARTESIAN_POINT ( 'NONE',  ( 85.15643035625001289, -34.75312499938548427, 99.99999999999998579 ) ) ;
#14923 = VECTOR ( 'NONE', #8838, 1000.000000000000000 ) ;
#14924 = CARTESIAN_POINT ( 'NONE',  ( -81.02178482187500208, -34.00312499938548427, -102.3871387122750889 ) ) ;
#14925 = CARTESIAN_POINT ( 'NONE',  ( 231.7961524227065979, -33.45134618820330275, -47.00000000000012079 ) ) ;
#14926 = CARTESIAN_POINT ( 'NONE',  ( -83.90000000000000568, -32.26874999877097139, -102.5980762113533018 ) ) ;
#14927 = CARTESIAN_POINT ( 'NONE',  ( 231.2217848218749339, -32.42812499938548143, 102.3871387122750889 ) ) ;
#14928 = CARTESIAN_POINT ( 'NONE',  ( -82.39999999999999147, -32.76018749875868252, 96.53589838486223584 ) ) ;
#14929 = ADVANCED_FACE ( 'NONE', ( #11998 ), #13267, .F. ) ;
#14930 = CARTESIAN_POINT ( 'NONE',  ( -82.39999999999999147, -34.41562499938547859, 96.81714838363319586 ) ) ;
#14931 = CIRCLE ( 'NONE', #17746, 5.200000000000001066 ) ;
#14932 = CARTESIAN_POINT ( 'NONE',  ( -81.59615242270662350, -31.66740381056766651, 103.0000000000000000 ) ) ;
#14933 = CARTESIAN_POINT ( 'NONE',  ( 79.64356964374998427, -33.10312499938548569, 98.40857419181659793 ) ) ;
#14934 = DIRECTION ( 'NONE',  ( 1.000000000000000000, -0.000000000000000000, -2.407412430484046130E-31 ) ) ;
#14935 = CARTESIAN_POINT ( 'NONE',  ( 85.40000000000000568, -33.99374999877097281, -99.99999999999998579 ) ) ;
#14936 = CARTESIAN_POINT ( 'NONE',  ( 234.0999999999999375, -32.54999999999999716, 102.5980762113533018 ) ) ;
#14937 = ORIENTED_EDGE ( 'NONE', *, *, #15830, .F. ) ;
#14938 = CARTESIAN_POINT ( 'NONE',  ( 235.3564303562499447, -34.07812499938548001, -50.00000000000011369 ) ) ;
#14939 = DIRECTION ( 'NONE',  ( 1.000000000000000000, 0.000000000000000000, 0.000000000000000000 ) ) ;
#14940 = CARTESIAN_POINT ( 'NONE',  ( 231.0999999999999375, -34.36874999877096570, 102.5980762113533018 ) ) ;
#14941 = CARTESIAN_POINT ( 'NONE',  ( 231.0999999999999375, -33.16874999877095576, -52.59807621135342970 ) ) ;
#14942 = CARTESIAN_POINT ( 'NONE',  ( -82.39999999999999147, -34.52812499938548285, 103.1828516163667899 ) ) ;
#14943 = ORIENTED_EDGE ( 'NONE', *, *, #9865, .F. ) ;
#14944 = ORIENTED_EDGE ( 'NONE', *, *, #8764, .F. ) ;
#14945 = CARTESIAN_POINT ( 'NONE',  ( -79.39999999999999147, -34.23750000000000426, -101.7320508075688963 ) ) ;
#14946 = CARTESIAN_POINT ( 'NONE',  ( -4.197312064133472020, -0.8182229787990021874, -3.502518405183886685 ) ) ;
#14947 = CARTESIAN_POINT ( 'NONE',  ( -81.59615242270665192, -34.81740381056767575, 103.0000000000000000 ) ) ;
#14948 = ORIENTED_EDGE ( 'NONE', *, *, #16774, .F. ) ;
#14949 = CARTESIAN_POINT ( 'NONE',  ( -82.49978216248248941, -34.99999999999999289, 102.7603866155199199 ) ) ;
#14950 = CARTESIAN_POINT ( 'NONE',  ( -82.40000000000001990, -33.65624999877097423, 97.00000000000000000 ) ) ;
#14951 = CARTESIAN_POINT ( 'NONE',  ( -79.64356964375001269, -33.14062499938548711, 98.40857419181659793 ) ) ;
#14952 = CARTESIAN_POINT ( 'NONE',  ( -85.40000000000000568, -34.53750000000000142, 98.26794919243111792 ) ) ;
#14953 = CARTESIAN_POINT ( 'NONE',  ( -80.90000000000000568, -32.34374999877096712, 97.40192378864668399 ) ) ;
#14954 = DIRECTION ( 'NONE',  ( 0.000000000000000000, -1.000000000000000000, 0.000000000000000000 ) ) ;
#14955 = FILL_AREA_STYLE ('',( #2164 ) ) ;
#14956 = CARTESIAN_POINT ( 'NONE',  ( 0.000000000000000000, 0.000000000000000000, -5.000000000000000000 ) ) ;
#14957 = CARTESIAN_POINT ( 'NONE',  ( -79.67114894419044901, -34.99999999999999289, -100.7768843408768760 ) ) ;
#14958 = CARTESIAN_POINT ( 'NONE',  ( 229.8435696437499303, -30.59062499938547575, 99.99999999999998579 ) ) ;
#14959 = ORIENTED_EDGE ( 'NONE', *, *, #15807, .T. ) ;
#14960 =( NAMED_UNIT ( * ) SI_UNIT ( $, .STERADIAN. ) SOLID_ANGLE_UNIT ( ) );
#14961 = CARTESIAN_POINT ( 'NONE',  ( -85.15643035624999868, -32.87812499938549138, -101.5914258081833879 ) ) ;
#14962 = CARTESIAN_POINT ( 'NONE',  ( -83.90000000000000568, -33.67500000000000426, 97.40192378864668399 ) ) ;
#14963 = EDGE_CURVE ( 'NONE', #13113, #13667, #3009, .T. ) ;
#14964 = ADVANCED_FACE ( 'NONE', ( #16401 ), #4679, .F. ) ;
#14965 = DIRECTION ( 'NONE',  ( 0.000000000000000000, 0.000000000000000000, -1.000000000000000000 ) ) ;
#14966 = CARTESIAN_POINT ( 'NONE',  ( 232.5999999999999375, -34.55624999877095860, 97.00000000000000000 ) ) ;
#14967 = CARTESIAN_POINT ( 'NONE',  ( -82.39999999999999147, -35.09062499938548285, 103.1828516163667899 ) ) ;
#14968 = CARTESIAN_POINT ( 'NONE',  ( 85.40000000000000568, -33.14999999999999858, -99.99999999999998579 ) ) ;
#14969 = CARTESIAN_POINT ( 'NONE',  ( 233.9782151781249411, -33.59062499938547575, -47.61286128772501769 ) ) ;
#14970 = ORIENTED_EDGE ( 'NONE', *, *, #7133, .T. ) ;
#14971 = ORIENTED_EDGE ( 'NONE', *, *, #756, .F. ) ;
#14972 = DIRECTION ( 'NONE',  ( -4.625929269271494788E-16, -1.000000000000000000, 0.000000000000000000 ) ) ;
#14973 = CARTESIAN_POINT ( 'NONE',  ( -82.39999999999999147, -30.11250000000000426, 96.53589838486223584 ) ) ;
#14974 = EDGE_CURVE ( 'NONE', #5649, #14237, #3200, .T. ) ;
#14975 = CARTESIAN_POINT ( 'NONE',  ( -83.90000000000000568, -31.66874999877096997, 102.5980762113533018 ) ) ;
#14976 = CARTESIAN_POINT ( 'NONE',  ( 82.39999999999999147, -31.91250000000000497, 103.4641016151377499 ) ) ;
#14977 = LINE ( 'NONE', #10386, #4634 ) ;
#14978 = CARTESIAN_POINT ( 'NONE',  ( 233.9782151781249411, -33.14062499938548001, 102.3871387122750889 ) ) ;
#14979 = CARTESIAN_POINT ( 'NONE',  ( 229.8435696437499303, -33.29062499938547148, -50.00000000000011369 ) ) ;
#14980 = CYLINDRICAL_SURFACE ( 'NONE', #7125, 3.000000000000002665 ) ;
#14981 = CARTESIAN_POINT ( 'NONE',  ( 85.15643035624999868, -31.90312499938548285, -101.5914258081833879 ) ) ;
#14982 = VERTEX_POINT ( 'NONE', #18159 ) ;
#14984 = ADVANCED_FACE ( 'NONE', ( #4386 ), #4782, .F. ) ;
#14983 = CARTESIAN_POINT ( 'NONE',  ( 235.5999999999999943, -31.16249999999999432, -48.26794919243124582 ) ) ;
#14985 = CARTESIAN_POINT ( 'NONE',  ( -82.40000000000000568, -31.63124999877096855, 102.9999999999999858 ) ) ;
#14986 = CARTESIAN_POINT ( 'NONE',  ( 85.15643035625001289, -32.39062499938548711, -99.99999999999998579 ) ) ;
#14987 = EDGE_CURVE ( 'NONE', #13520, #13113, #855, .T. ) ;
#14988 = CARTESIAN_POINT ( 'NONE',  ( 0.000000000000000000, 0.000000000000000000, -4.000000000000000000 ) ) ;
#14989 = CARTESIAN_POINT ( 'NONE',  ( 79.39999999999999147, -33.78750000000000853, -98.26794919243110371 ) ) ;
#14990 = CARTESIAN_POINT ( 'NONE',  ( 229.8435696437499303, -30.25312499938548072, -50.00000000000011369 ) ) ;
#14991 = EDGE_CURVE ( 'NONE', #11600, #12396, #16502, .T. ) ;
#14992 = CARTESIAN_POINT ( 'NONE',  ( -85.15643035625001289, -34.64062499938548711, 99.99999999999998579 ) ) ;
#14993 = ORIENTED_EDGE ( 'NONE', *, *, #11010, .T. ) ;
#14994 = LINE ( 'NONE', #5727, #6509 ) ;
#14995 = SHAPE_REPRESENTATION ( 'connecting block', ( #10540 ), #5560 ) ;
#14996 = CARTESIAN_POINT ( 'NONE',  ( 229.8435696437499587, -33.77812499938547575, 98.40857419181659793 ) ) ;
#14997 = DIRECTION ( 'NONE',  ( 1.000000000000000000, 0.000000000000000000, 0.000000000000000000 ) ) ;
#14998 = CARTESIAN_POINT ( 'NONE',  ( -85.40000000000000568, -32.20856250001229171, 101.7320508075688679 ) ) ;
#14999 = CARTESIAN_POINT ( 'NONE',  ( -82.40000000000000568, -33.03750000000000142, -96.99999999999998579 ) ) ;
#15000 = EDGE_CURVE ( 'NONE', #10326, #540, #1986, .T. ) ;
#15001 = CARTESIAN_POINT ( 'NONE',  ( 109.9999999999999432, -29.80000000000003268, -130.0000000000000000 ) ) ;
#15002 = CARTESIAN_POINT ( 'NONE',  ( -83.77821517812500929, -31.86562499938548498, 102.3871387122750889 ) ) ;
#15003 = CARTESIAN_POINT ( 'NONE',  ( 229.6880761451935484, -34.99999999999999289, 99.60674545263957214 ) ) ;
#15004 = CARTESIAN_POINT ( 'NONE',  ( 85.15643035624999868, -31.56562499938548427, 98.40857419181659793 ) ) ;
#15005 = CARTESIAN_POINT ( 'NONE',  ( -83.90000000000000568, -32.62500000000000000, 102.5980762113533018 ) ) ;
#15006 = CARTESIAN_POINT ( 'NONE',  ( -80.90000000000000568, -32.55000000000000426, -97.40192378864668399 ) ) ;
#15007 = CARTESIAN_POINT ( 'NONE',  ( -84.85729912020875076, -32.00000000000000000, -98.73859666561340021 ) ) ;
#15008 = CARTESIAN_POINT ( 'NONE',  ( -85.15643035624999868, -30.66562499938548569, -98.40857419181659793 ) ) ;
#15009 = ORIENTED_EDGE ( 'NONE', *, *, #757, .T. ) ;
#15010 = CARTESIAN_POINT ( 'NONE',  ( 83.90000000000000568, -34.51874999877097139, 102.5980762113533018 ) ) ;
#15011 = CARTESIAN_POINT ( 'NONE',  ( 1.734723475976807094E-15, 4.618802153517012954, -0.4999999999999995559 ) ) ;
#15012 = CARTESIAN_POINT ( 'NONE',  ( -79.68596062386970402, -32.00000000000002132, 101.2782762865727619 ) ) ;
#15013 = CARTESIAN_POINT ( 'NONE',  ( -79.64356964375001269, -32.69062499938548427, 98.40857419181659793 ) ) ;
#15014 = CARTESIAN_POINT ( 'NONE',  ( 81.44903907897412410, -31.99999999999999289, 102.7404298451301514 ) ) ;
#15015 = VERTEX_POINT ( 'NONE', #6433 ) ;
#15016 = ADVANCED_FACE ( 'NONE', ( #7889 ), #4975, .T. ) ;
#15017 = CARTESIAN_POINT ( 'NONE',  ( -82.39999999999999147, -31.91250000000000497, -103.4641016151377499 ) ) ;
#15018 = CARTESIAN_POINT ( 'NONE',  ( 3.878104551856474735, -0.7018542299754126912, -3.499999999999999556 ) ) ;
#15019 = LINE ( 'NONE', #12181, #19206 ) ;
#15020 = CARTESIAN_POINT ( 'NONE',  ( -79.64356964374999848, -34.07812499938548711, -99.99999999999998579 ) ) ;
#15021 = LINE ( 'NONE', #1641, #10496 ) ;
#15022 = CARTESIAN_POINT ( 'NONE',  ( 235.3564303562499447, -32.24062499938548143, 98.40857419181659793 ) ) ;
#15023 = CARTESIAN_POINT ( 'NONE',  ( -82.39999999999999147, -32.31018749875868679, 96.53589838486223584 ) ) ;
#15024 = CARTESIAN_POINT ( 'NONE',  ( -81.02178482187500208, -32.65312499938548996, 97.61286128772489690 ) ) ;
#15025 = CARTESIAN_POINT ( 'NONE',  ( -79.64356964374998427, -33.92812499938548854, -101.5914258081833879 ) ) ;
#15026 = CARTESIAN_POINT ( 'NONE',  ( 79.64356964374998427, -33.47812499938547859, 101.5914258081833879 ) ) ;
#15027 = DIRECTION ( 'NONE',  ( 0.000000000000000000, 0.000000000000000000, -1.000000000000000000 ) ) ;
#15028 = CARTESIAN_POINT ( 'NONE',  ( 83.20384757729335945, -32.60759618943233562, -102.9999999999999858 ) ) ;
#15029 = CARTESIAN_POINT ( 'NONE',  ( 83.90000000000000568, -33.46874999877096712, -102.5980762113533018 ) ) ;
#15030 = CARTESIAN_POINT ( 'NONE',  ( 229.5999999999999375, -34.04999999999999716, 99.99999999999998579 ) ) ;
#15031 = VERTEX_POINT ( 'NONE', #17071 ) ;
#15032 = CARTESIAN_POINT ( 'NONE',  ( 232.5999999999999943, -32.39062499938548001, -46.81714838363331666 ) ) ;
#15033 = CARTESIAN_POINT ( 'NONE',  ( 233.9782151781249411, -30.85312499938547859, 97.61286128772489690 ) ) ;
#15034 = CARTESIAN_POINT ( 'NONE',  ( 235.5999999999999375, -32.86874999877096570, -50.00000000000011369 ) ) ;
#15035 = CARTESIAN_POINT ( 'NONE',  ( -85.15643035625001289, -33.25312499938548427, 101.5914258081833879 ) ) ;
#15036 = ORIENTED_EDGE ( 'NONE', *, *, #3390, .T. ) ;
#15037 = ORIENTED_EDGE ( 'NONE', *, *, #6848, .T. ) ;
#15038 = CARTESIAN_POINT ( 'NONE',  ( 4.154306624730864428, 2.398490048084778170, -3.721999068284300272 ) ) ;
#15039 = CARTESIAN_POINT ( 'NONE',  ( -79.39999999999999147, -34.25624999877096855, 101.7320508075688537 ) ) ;
#15040 = DIRECTION ( 'NONE',  ( -0.000000000000000000, -1.000000000000000000, -0.000000000000000000 ) ) ;
#15041 = VERTEX_POINT ( 'NONE', #18257 ) ;
#15042 = DIRECTION ( 'NONE',  ( 0.000000000000000000, 0.000000000000000000, -1.000000000000000000 ) ) ;
#15043 = CARTESIAN_POINT ( 'NONE',  ( -82.39999999999999147, -31.85624999877096641, 96.99999999999998579 ) ) ;
#15044 = VECTOR ( 'NONE', #2931, 1000.000000000000000 ) ;
#15045 = CARTESIAN_POINT ( 'NONE',  ( -82.39999999999999147, -32.84062499938548996, 103.1828516163667899 ) ) ;
#15046 = CARTESIAN_POINT ( 'NONE',  ( -79.39999999999999147, -30.61874999877096926, 99.99999999999998579 ) ) ;
#15047 = CARTESIAN_POINT ( 'NONE',  ( -85.40000000000000568, -32.64374999877097139, 99.99999999999998579 ) ) ;
#15048 = CARTESIAN_POINT ( 'NONE',  ( 231.0999999999999375, -33.52499999999999147, 102.5980762113533018 ) ) ;
#15049 = CARTESIAN_POINT ( 'NONE',  ( -82.39999999999999147, -31.01249999999999929, 96.99999999999998579 ) ) ;
#15050 = DIRECTION ( 'NONE',  ( 1.735459783503185124E-31, 3.491481338843133355E-15, 1.000000000000000000 ) ) ;
#15051 = CARTESIAN_POINT ( 'NONE',  ( 3.999999999999999112, -0.3979232138631231819, -5.929230630780099908E-17 ) ) ;
#15052 = CARTESIAN_POINT ( 'NONE',  ( 229.8435696437499871, -31.97812499938548214, 98.40857419181659793 ) ) ;
#15053 = ORIENTED_EDGE ( 'NONE', *, *, #18718, .F. ) ;
#15054 = CARTESIAN_POINT ( 'NONE',  ( -79.64356964375001269, -34.37812499938548427, -101.5914258081833879 ) ) ;
#15055 = CARTESIAN_POINT ( 'NONE',  ( 0.5636800770130377947, 4.293361309317166530, -3.531542292954102713 ) ) ;
#15056 = VECTOR ( 'NONE', #17525, 1000.000000000000000 ) ;
#15057 = PRESENTATION_LAYER_ASSIGNMENT (  '', '', ( #6011 ) ) ;
#15058 = CARTESIAN_POINT ( 'NONE',  ( 232.5999999999999375, -34.55624999877095860, -53.00000000000011369 ) ) ;
#15059 = CARTESIAN_POINT ( 'NONE',  ( -83.90000000000000568, -32.56874999877096855, 102.5980762113533018 ) ) ;
#15060 = CARTESIAN_POINT ( 'NONE',  ( -85.15643035624999868, -33.77812499938548285, 98.40857419181659793 ) ) ;
#15061 = CARTESIAN_POINT ( 'NONE',  ( 230.9316747517381430, -35.00000000000000000, -47.74327260034019105 ) ) ;
#15062 = CYLINDRICAL_SURFACE ( 'NONE', #17886, 5.199999999999996625 ) ;
#15063 = EDGE_LOOP ( 'NONE', ( #14741, #7542, #17374, #16317 ) ) ;
#15064 = ORIENTED_EDGE ( 'NONE', *, *, #6390, .F. ) ;
#15065 = CARTESIAN_POINT ( 'NONE',  ( -84.93334430221554499, -32.00000000000000000, 101.1009827666099596 ) ) ;
#15066 = CARTESIAN_POINT ( 'NONE',  ( -80.90000000000000568, -31.20000000000000284, 102.5980762113533018 ) ) ;
#15067 = CARTESIAN_POINT ( 'NONE',  ( -85.40000000000000568, -30.88124999877097210, 98.26794919243111792 ) ) ;
#15068 = CARTESIAN_POINT ( 'NONE',  ( 82.39999999999999147, -31.01249999999999929, 103.4641016151377499 ) ) ;
#15069 = DIRECTION ( 'NONE',  ( -0.000000000000000000, 0.000000000000000000, -1.000000000000000000 ) ) ;
#15071 = CARTESIAN_POINT ( 'NONE',  ( 229.8435696437499871, -34.60312499938547859, 101.5914258081833879 ) ) ;
#15070 = AXIS2_PLACEMENT_3D ( 'NONE', #1596, #14972, #9012 ) ;
#15072 = CARTESIAN_POINT ( 'NONE',  ( 231.2217848218749339, -34.56562499938547717, -47.61286128772501769 ) ) ;
#15073 = CARTESIAN_POINT ( 'NONE',  ( 81.44903907892005179, -31.99999999999999289, -97.25957015488572210 ) ) ;
#15074 = ADVANCED_FACE ( 'NONE', ( #767 ), #8086, .T. ) ;
#15075 = CARTESIAN_POINT ( 'NONE',  ( 85.15643035625001289, -31.04062499938548569, -99.99999999999998579 ) ) ;
#15076 = ORIENTED_EDGE ( 'NONE', *, *, #5603, .F. ) ;
#15077 = CARTESIAN_POINT ( 'NONE',  ( 231.0999999999999375, -32.62499999999999289, -47.40192378864679768 ) ) ;
#15078 = CARTESIAN_POINT ( 'NONE',  ( -99.99999999999998579, -3.000000000000000000, 150.0000000000000000 ) ) ;
#15079 = CARTESIAN_POINT ( 'NONE',  ( 81.02178482187500208, -32.99062499938548854, -97.61286128772489690 ) ) ;
#15080 = EDGE_CURVE ( 'NONE', #14762, #15086, #15218, .T. ) ;
#15081 = ADVANCED_FACE ( 'NONE', ( #13839 ), #3486, .F. ) ;
#15082 = CYLINDRICAL_SURFACE ( 'NONE', #15678, 2.649999999999985700 ) ;
#15083 = CARTESIAN_POINT ( 'NONE',  ( -82.40000000000001990, -34.61250000000001137, 97.00000000000000000 ) ) ;
#15084 = CARTESIAN_POINT ( 'NONE',  ( 233.9782151781249411, -30.55312499938548143, -47.61286128772501769 ) ) ;
#15085 = CARTESIAN_POINT ( 'NONE',  ( -83.90000000000000568, -30.07499999999999929, 97.40192378864668399 ) ) ;
#15086 = VERTEX_POINT ( 'NONE', #12666 ) ;
#15087 = CARTESIAN_POINT ( 'NONE',  ( -84.85538848574861959, -34.99999999999998579, 98.27756861399178945 ) ) ;
#15088 = CARTESIAN_POINT ( 'NONE',  ( 232.5999999999999375, -29.99999999999999645, -50.00000000000011369 ) ) ;
#15089 = CARTESIAN_POINT ( 'NONE',  ( 79.64356964374999848, -31.26562499938548356, 99.99999999999998579 ) ) ;
#15090 = CARTESIAN_POINT ( 'NONE',  ( -82.39999999999999147, -33.03356250001230165, 103.4641016151377499 ) ) ;
#15091 = EDGE_CURVE ( 'NONE', #11038, #14982, #7971, .T. ) ;
#15092 = CARTESIAN_POINT ( 'NONE',  ( 0.6448876103708359731, 4.246476118072354922, -0.2256878752776725616 ) ) ;
#15093 = EDGE_CURVE ( 'NONE', #17308, #8302, #9903, .T. ) ;
#15094 = CARTESIAN_POINT ( 'NONE',  ( -81.02178482187500208, -30.55312499938548854, 102.3871387122750889 ) ) ;
#15095 = CARTESIAN_POINT ( 'NONE',  ( 235.5999999999999375, -32.02499999999999858, 99.99999999999998579 ) ) ;
#15096 = CARTESIAN_POINT ( 'NONE',  ( 85.15643035624999868, -34.71562499938548285, 98.40857419181659793 ) ) ;
#15097 = EDGE_CURVE ( 'NONE', #10928, #15550, #12574, .T. ) ;
#15098 = PLANE ( 'NONE',  #16149 ) ;
#15099 = CARTESIAN_POINT ( 'NONE',  ( 235.3564303562499447, -30.36562499938547788, -50.00000000000011369 ) ) ;
#15100 = CARTESIAN_POINT ( 'NONE',  ( -84.93334430221560183, -32.00000000000000711, -98.89901723339004036 ) ) ;
#15101 = DIRECTION ( 'NONE',  ( -0.000000000000000000, -0.000000000000000000, 1.000000000000000000 ) ) ;
#15102 = ORIENTED_EDGE ( 'NONE', *, *, #17357, .T. ) ;
#15103 = CARTESIAN_POINT ( 'NONE',  ( 85.40000000000000568, -34.40624999877096712, 98.26794919243111792 ) ) ;
#15104 = CARTESIAN_POINT ( 'NONE',  ( 85.40000000000000568, -34.44374999877096855, 99.99999999999998579 ) ) ;
#15105 =( BOUNDED_CURVE ( )  B_SPLINE_CURVE ( 2, ( #3638, #12915, #5211, #3926, #9600, #11158, #15564, #11353, #9794 ),
 .UNSPECIFIED., .F., .F. ) 
 B_SPLINE_CURVE_WITH_KNOTS ( ( 3, 2, 2, 2, 3 ),
 ( 0.6041666666666666297, 0.6111111111111111605, 0.6250000000000000000, 0.6388888888888888395, 0.6458333333333333703 ),
 .UNSPECIFIED. ) 
 CURVE ( )  GEOMETRIC_REPRESENTATION_ITEM ( )  RATIONAL_B_SPLINE_CURVE ( ( 0.9330127018922192983, 0.9330127018922187432, 1.000000000000000000, 0.8660254037844387076, 1.000000000000000000, 0.8660254037844387076, 1.000000000000000000, 0.9330127018922187432, 0.9330127018922192983 ) ) 
 REPRESENTATION_ITEM ( '' )  );
#15106 = CARTESIAN_POINT ( 'NONE',  ( -82.39999999999999147, -30.81562499938548427, 96.81714838363319586 ) ) ;
#15107 = DIRECTION ( 'NONE',  ( 0.000000000000000000, -1.000000000000000000, 0.000000000000000000 ) ) ;
#15108 = VERTEX_POINT ( 'NONE', #9652 ) ;
#15109 = CARTESIAN_POINT ( 'NONE',  ( -80.90000000000000568, -30.15000000000000213, -102.5980762113533018 ) ) ;
#15110 = DIRECTION ( 'NONE',  ( 0.000000000000000000, 0.000000000000000000, 1.000000000000000000 ) ) ;
#15111 = CARTESIAN_POINT ( 'NONE',  ( -85.40000000000000568, -34.85624999877096997, -98.26794919243111792 ) ) ;
#15112 = CARTESIAN_POINT ( 'NONE',  ( -85.15643035625001289, -33.85312499938549280, -99.99999999999998579 ) ) ;
#15113 = CARTESIAN_POINT ( 'NONE',  ( -2.836893136758495970, -3.208949435745868328, -3.505054077164885484 ) ) ;
#15114 = CARTESIAN_POINT ( 'NONE',  ( 235.3564303562499447, -34.49062499938548143, 98.40857419181659793 ) ) ;
#15115 = CARTESIAN_POINT ( 'NONE',  ( -85.40000000000000568, -31.29768749875867684, 99.99999999999998579 ) ) ;
#15116 = ORIENTED_EDGE ( 'NONE', *, *, #7661, .F. ) ;
#15117 = CARTESIAN_POINT ( 'NONE',  ( -81.02178482187500208, -33.25312499938548427, 102.3871387122750889 ) ) ;
#15118 = CARTESIAN_POINT ( 'NONE',  ( -83.20384757729335945, -33.45134618820330985, 102.9999999999999858 ) ) ;
#15119 = CARTESIAN_POINT ( 'NONE',  ( 79.64356964374998427, -33.92812499938548854, 101.5914258081833879 ) ) ;
#15120 = LINE ( 'NONE', #6338, #17111 ) ;
#15121 = EDGE_CURVE ( 'NONE', #4621, #12012, #6789, .T. ) ;
#15122 = CARTESIAN_POINT ( 'NONE',  ( 5.599999999999999645, -2.020725942163695166, -3.500000000000000000 ) ) ;
#15123 = ADVANCED_FACE ( 'NONE', ( #11104, #386 ), #18352, .F. ) ;
#15124 = CARTESIAN_POINT ( 'NONE',  ( 85.40000000000000568, -34.44374999877096855, -99.99999999999998579 ) ) ;
#15125 = CARTESIAN_POINT ( 'NONE',  ( 234.0999999999999375, -33.89999999999999147, 102.5980762113533018 ) ) ;
#15126 = VERTEX_POINT ( 'NONE', #12385 ) ;
#15127 = CARTESIAN_POINT ( 'NONE',  ( 232.5999999999999943, -34.19062499938547717, -46.81714838363331666 ) ) ;
#15128 = DIRECTION ( 'NONE',  ( 1.000000000000000000, 0.000000000000000000, 0.000000000000000000 ) ) ;
#15129 = CARTESIAN_POINT ( 'NONE',  ( 229.5999999999999375, -34.48124999877096286, 98.26794919243111792 ) ) ;
#15130 = CARTESIAN_POINT ( 'NONE',  ( 234.0999999999999375, -35.19374999877096855, -47.40192378864679768 ) ) ;
#15131 = CARTESIAN_POINT ( 'NONE',  ( -84.70388354820684640, -35.00002705695768412, 98.07851859032987818 ) ) ;
#15132 = ORIENTED_EDGE ( 'NONE', *, *, #19273, .F. ) ;
#15134 = ORIENTED_EDGE ( 'NONE', *, *, #9224, .T. ) ;
#15133 = ADVANCED_FACE ( 'NONE', ( #7984 ), #13939, .F. ) ;
#15135 = CARTESIAN_POINT ( 'NONE',  ( -85.15643035625001289, -30.14062499938548711, -99.99999999999998579 ) ) ;
#15136 = CARTESIAN_POINT ( 'NONE',  ( -4.204114297095464359, 1.660363174096617156, -3.602136431857887011 ) ) ;
#15137 = VERTEX_POINT ( 'NONE', #12478 ) ;
#15138 = CYLINDRICAL_SURFACE ( 'NONE', #2649, 3.000000000000002665 ) ;
#15139 = FACE_BOUND ( 'NONE', #12137, .T. ) ;
#15140 = AXIS2_PLACEMENT_3D ( 'NONE', #19231, #1160, #19131 ) ;
#15141 = CARTESIAN_POINT ( 'NONE',  ( -83.77821517812500929, -34.82812499938548711, 97.61286128772489690 ) ) ;
#15142 = CARTESIAN_POINT ( 'NONE',  ( -85.40000000000000568, -33.63750000000000284, 98.26794919243111792 ) ) ;
#15143 = CARTESIAN_POINT ( 'NONE',  ( -82.39999999999999147, -31.40624999877097068, 96.53589838486223584 ) ) ;
#15144 = DIRECTION ( 'NONE',  ( 0.000000000000000000, 0.000000000000000000, -1.000000000000000000 ) ) ;
#15145 = FACE_OUTER_BOUND ( 'NONE', #6471, .T. ) ;
#15146 = LINE ( 'NONE', #4897, #8051 ) ;
#15147 = CARTESIAN_POINT ( 'NONE',  ( 244.7999999999999545, -29.80000000000002203, 147.7999999999999829 ) ) ;
#15148 = CARTESIAN_POINT ( 'NONE',  ( 229.8435696437499871, -31.45312499938547290, 101.5914258081833879 ) ) ;
#15149 = ORIENTED_EDGE ( 'NONE', *, *, #14847, .F. ) ;
#15150 = CARTESIAN_POINT ( 'NONE',  ( -79.64356964374999848, -33.06562499938548427, -99.99999999999998579 ) ) ;
#15151 = CARTESIAN_POINT ( 'NONE',  ( 231.7961524227065695, -32.28615380933862156, 96.99999999999997158 ) ) ;
#15152 = VECTOR ( 'NONE', #14798, 1000.000000000000000 ) ;
#15153 = DIRECTION ( 'NONE',  ( 1.000000000000000000, 0.000000000000000000, -0.000000000000000000 ) ) ;
#15154 = CARTESIAN_POINT ( 'NONE',  ( 82.39999999999999147, -33.20624999877097849, -97.00000000000000000 ) ) ;
#15155 = CARTESIAN_POINT ( 'NONE',  ( 4.000000000000000000, 0.1981133338132474442, 2.382280164152719704E-17 ) ) ;
#15156 = CARTESIAN_POINT ( 'NONE',  ( 229.8435696437499871, -34.15312499938547575, -48.40857419181671162 ) ) ;
#15157 = EDGE_LOOP ( 'NONE', ( #3108, #6089, #13146, #3014 ) ) ;
#15158 = ORIENTED_EDGE ( 'NONE', *, *, #16190, .T. ) ;
#15159 = CARTESIAN_POINT ( 'NONE',  ( 79.39999999999999147, -34.70624999877097139, 98.26794919243113213 ) ) ;
#15160 = CARTESIAN_POINT ( 'NONE',  ( -80.90000000000000568, -30.30000000000000426, 102.5980762113533018 ) ) ;
#15161 = CARTESIAN_POINT ( 'NONE',  ( -80.90000000000000568, -32.49374999877097281, 102.5980762113533018 ) ) ;
#15162 = CARTESIAN_POINT ( 'NONE',  ( 80.90000000000000568, -31.65000000000000568, 97.40192378864668399 ) ) ;
#15163 = LINE ( 'NONE', #12041, #8988 ) ;
#15164 = CARTESIAN_POINT ( 'NONE',  ( 233.9782151781249411, -33.59062499938547575, 102.3871387122750889 ) ) ;
#15165 = AXIS2_PLACEMENT_3D ( 'NONE', #9543, #765, #16880 ) ;
#15166 = CARTESIAN_POINT ( 'NONE',  ( 79.64356964374999848, -33.62812499938548427, -99.99999999999998579 ) ) ;
#15167 = EDGE_CURVE ( 'NONE', #15882, #17789, #6730, .T. ) ;
#15168 = DIRECTION ( 'NONE',  ( 0.000000000000000000, -1.000000000000000000, 0.000000000000000000 ) ) ;
#15169 = CARTESIAN_POINT ( 'NONE',  ( 79.64356964375001269, -33.02812499938548285, -98.40857419181659793 ) ) ;
#15170 = EDGE_LOOP ( 'NONE', ( #5349, #6148, #7700, #16358 ) ) ;
#15171 = CARTESIAN_POINT ( 'NONE',  ( 229.5999999999999375, -33.63749999999998863, -51.73205080756898866 ) ) ;
#15172 = CARTESIAN_POINT ( 'NONE',  ( 82.39999999999999147, -34.07812499938548711, -103.1828516163667899 ) ) ;
#15173 = CARTESIAN_POINT ( 'NONE',  ( 82.39999999999999147, -32.72812499938548569, -103.1828516163667899 ) ) ;
#15174 = PRESENTATION_LAYER_ASSIGNMENT (  '', '', ( #14853 ) ) ;
#15175 = FACE_OUTER_BOUND ( 'NONE', #287, .T. ) ;
#15176 = CARTESIAN_POINT ( 'NONE',  ( -82.39999999999999147, -32.16562499938549280, 96.81714838363319586 ) ) ;
#15177 = CARTESIAN_POINT ( 'NONE',  ( 235.3564303562499447, -34.11562499938548143, -48.40857419181671162 ) ) ;
#15178 = CARTESIAN_POINT ( 'NONE',  ( -82.39999999999999147, -34.97812499938547859, 103.1828516163667899 ) ) ;
#15179 = ORIENTED_EDGE ( 'NONE', *, *, #8646, .F. ) ;
#15180 = CARTESIAN_POINT ( 'NONE',  ( -84.23541345008663939, -34.99840151550829859, 102.3957176879168713 ) ) ;
#15181 = CARTESIAN_POINT ( 'NONE',  ( 85.15643035625001289, -30.59062499938548285, 99.99999999999998579 ) ) ;
#15182 = EDGE_CURVE ( 'NONE', #11132, #17929, #8157, .T. ) ;
#15183 = EDGE_CURVE ( 'NONE', #15647, #6543, #19116, .T. ) ;
#15184 = CARTESIAN_POINT ( 'NONE',  ( 230.0213320530828582, -31.99999999999997868, -50.98998077060178247 ) ) ;
#15185 = CARTESIAN_POINT ( 'NONE',  ( -85.15643035625001289, -31.11562499938548143, 101.5914258081833879 ) ) ;
#15186 = AXIS2_PLACEMENT_3D ( 'NONE', #5953, #12190, #8967 ) ;
#15187 = CARTESIAN_POINT ( 'NONE',  ( -82.40000000000000568, -33.03750000000000142, 102.9999999999999858 ) ) ;
#15188 = CARTESIAN_POINT ( 'NONE',  ( 85.15643035624999868, -35.22676555956768141, 101.0032586025029815 ) ) ;
#15189 = CARTESIAN_POINT ( 'NONE',  ( 79.64356964375001269, -30.96562499938548640, -101.5914258081833879 ) ) ;
#15190 = CARTESIAN_POINT ( 'NONE',  ( 235.3564303562499447, -30.40312499938547575, -48.40857419181671162 ) ) ;
#15191 = DIRECTION ( 'NONE',  ( -0.000000000000000000, -1.000000000000000000, -0.000000000000000000 ) ) ;
#15192 = CARTESIAN_POINT ( 'NONE',  ( -85.15643035625001289, -32.50312499938548427, -99.99999999999998579 ) ) ;
#15193 = ORIENTED_EDGE ( 'NONE', *, *, #695, .T. ) ;
#15194 = CARTESIAN_POINT ( 'NONE',  ( 83.90000000000000568, -34.36874999877097281, 97.40192378864668399 ) ) ;
#15195 = AXIS2_PLACEMENT_3D ( 'NONE', #7921, #9380, #331 ) ;
#15196 = CARTESIAN_POINT ( 'NONE',  ( -83.20384757729337366, -33.18615380933864145, 97.00000000000000000 ) ) ;
#15197 = CARTESIAN_POINT ( 'NONE',  ( 4.093692494532767512, -2.021783646005781421, -3.501831996793853374 ) ) ;
#15198 = EDGE_CURVE ( 'NONE', #18970, #5195, #3984, .T. ) ;
#15199 = CARTESIAN_POINT ( 'NONE',  ( -82.39999999999999147, -32.39062499938548001, 103.1828516163667899 ) ) ;
#15200 = CARTESIAN_POINT ( 'NONE',  ( 82.40000000000000568, -30.00000000000000355, -96.99999999999998579 ) ) ;
#15201 = ORIENTED_EDGE ( 'NONE', *, *, #9496, .F. ) ;
#15202 = CARTESIAN_POINT ( 'NONE',  ( -80.90000000000000568, -32.10000000000000142, -97.40192378864668399 ) ) ;
#15203 = VECTOR ( 'NONE', #14164, 1000.000000000000000 ) ;
#15204 = COLOUR_RGB ( '',0.8941176470588234615, 0.8941176470588234615, 0.8941176470588234615 ) ;
#15205 = CARTESIAN_POINT ( 'NONE',  ( 85.40000000000000568, -34.53750000000000142, -98.26794919243111792 ) ) ;
#15206 = CARTESIAN_POINT ( 'NONE',  ( -6.473970235329672780E-16, -4.862606272033106691, -3.745885042887442395 ) ) ;
#15207 = CARTESIAN_POINT ( 'NONE',  ( 79.68596062386910717, -31.99999999999998579, -101.2782762865714972 ) ) ;
#15208 = CARTESIAN_POINT ( 'NONE',  ( 232.5999999999999375, -33.65624999877096002, 97.00000000000000000 ) ) ;
#15209 = EDGE_CURVE ( 'NONE', #12222, #7898, #18930, .T. ) ;
#15210 = CARTESIAN_POINT ( 'NONE',  ( 232.5999999999999375, -34.64062499938548001, 103.1828516163667899 ) ) ;
#15211 = CARTESIAN_POINT ( 'NONE',  ( -85.40000000000000568, -32.19768749875867542, 99.99999999999998579 ) ) ;
#15212 =( GEOMETRIC_REPRESENTATION_CONTEXT ( 3 ) GLOBAL_UNCERTAINTY_ASSIGNED_CONTEXT ( ( #14274 ) ) GLOBAL_UNIT_ASSIGNED_CONTEXT ( ( #533, #5319, #11259 ) ) REPRESENTATION_CONTEXT ( 'NONE', 'WORKASPACE' ) );
#15213 = EDGE_LOOP ( 'NONE', ( #7583, #14944, #12738, #18057, #1198, #6568 ) ) ;
#15214 = CARTESIAN_POINT ( 'NONE',  ( 232.5999999999999659, -32.58749999999999858, 102.9999999999999858 ) ) ;
#15215 = CARTESIAN_POINT ( 'NONE',  ( 85.40000000000000568, -32.28750000000000142, 101.7320508075688821 ) ) ;
#15216 = CARTESIAN_POINT ( 'NONE',  ( 81.02178482187500208, -32.99062499938548854, 102.3871387122750889 ) ) ;
#15217 = CARTESIAN_POINT ( 'NONE',  ( 82.40000000000000568, -34.55624999877097281, -97.00000000000000000 ) ) ;
#15218 = LINE ( 'NONE', #3398, #2402 ) ;
#15219 = CARTESIAN_POINT ( 'NONE',  ( 85.40000000000000568, -34.48124999877096997, -98.26794919243111792 ) ) ;
#15220 = AXIS2_PLACEMENT_3D ( 'NONE', #3225, #6271, #10462 ) ;
#15221 = CARTESIAN_POINT ( 'NONE',  ( -2.000000000000007550, -3.464101615137749945, 0.000000000000000000 ) ) ;
#15222 =( BOUNDED_CURVE ( )  B_SPLINE_CURVE ( 2, ( #10398, #16557, #10210, #3158, #1700, #1416, #4250, #154, #6105 ),
 .UNSPECIFIED., .F., .F. ) 
 B_SPLINE_CURVE_WITH_KNOTS ( ( 3, 2, 2, 2, 3 ),
 ( 0.7708333333333331483, 0.7777777777777777901, 0.7916666666666666297, 0.8055555555555555802, 0.8125000000000001110 ),
 .UNSPECIFIED. ) 
 CURVE ( )  GEOMETRIC_REPRESENTATION_ITEM ( )  RATIONAL_B_SPLINE_CURVE ( ( 0.9330127018922194093, 0.9330127018922177440, 1.000000000000000000, 0.8660254037844387076, 1.000000000000000000, 0.8660254037844387076, 1.000000000000000000, 0.9330127018922182991, 0.9330127018922194093 ) ) 
 REPRESENTATION_ITEM ( '' )  );
#15223 = CIRCLE ( 'NONE', #6815, 3.000000000000002665 ) ;
#15224 = ORIENTED_EDGE ( 'NONE', *, *, #17977, .T. ) ;
#15225 = CARTESIAN_POINT ( 'NONE',  ( 235.3564303562499447, -33.14062499938548001, -51.59142580818350154 ) ) ;
#15226 = DIRECTION ( 'NONE',  ( 1.000000000000000000, 0.000000000000000000, 0.000000000000000000 ) ) ;
#15227 = CARTESIAN_POINT ( 'NONE',  ( 229.5999999999999375, -35.34374999877096002, 99.99999999999998579 ) ) ;
#15228 = CARTESIAN_POINT ( 'NONE',  ( 231.2217848218749339, -30.77812499938548285, -52.38713871227520968 ) ) ;
#15229 = DIRECTION ( 'NONE',  ( -1.000000000000000000, 1.387778780781445676E-15, 2.407412430484046130E-31 ) ) ;
#15230 = VECTOR ( 'NONE', #12199, 1000.000000000000000 ) ;
#15231 = ORIENTED_EDGE ( 'NONE', *, *, #1234, .F. ) ;
#15232 = VERTEX_POINT ( 'NONE', #17652 ) ;
#15233 = CARTESIAN_POINT ( 'NONE',  ( -79.64356964374999848, -30.36562499938548498, -99.99999999999998579 ) ) ;
#15234 = DIRECTION ( 'NONE',  ( 0.000000000000000000, 0.000000000000000000, 1.000000000000000000 ) ) ;
#15235 = CARTESIAN_POINT ( 'NONE',  ( -83.20384757729335945, -34.14240381056767148, -102.9999999999999716 ) ) ;
#15236 = EDGE_LOOP ( 'NONE', ( #7206, #13869, #19027, #2064 ) ) ;
#15237 = DIRECTION ( 'NONE',  ( 2.312964634635736745E-15, 1.000000000000000000, 0.000000000000000000 ) ) ;
#15238 = CARTESIAN_POINT ( 'NONE',  ( 231.0999999999999375, -33.91874999877096286, 102.5980762113533018 ) ) ;
#15239 = AXIS2_PLACEMENT_3D ( 'NONE', #17675, #7982, #13938 ) ;
#15240 = CARTESIAN_POINT ( 'NONE',  ( -79.39999999999999147, -34.27499999999999858, 99.99999999999998579 ) ) ;
#15241 = CARTESIAN_POINT ( 'NONE',  ( -83.90000000000000568, -33.67500000000000426, 97.40192378864668399 ) ) ;
#15242 = CARTESIAN_POINT ( 'NONE',  ( -83.90000000000000568, -34.36874999877097281, 102.5980762113533018 ) ) ;
#15243 = DIRECTION ( 'NONE',  ( -1.000000000000000000, 1.224646799147352714E-16, 0.000000000000000000 ) ) ;
#15244 = DIRECTION ( 'NONE',  ( -1.000000000000000000, 0.000000000000000000, 0.000000000000000000 ) ) ;
#15245 = EDGE_CURVE ( 'NONE', #11020, #5276, #15708, .T. ) ;
#15246 = SURFACE_STYLE_USAGE ( .BOTH. , #12021 ) ;
#15247 = CARTESIAN_POINT ( 'NONE',  ( -80.90000000000000568, -33.30000000000000426, 97.40192378864668399 ) ) ;
#15248 = CARTESIAN_POINT ( 'NONE',  ( 231.2217848218749339, -35.01562499938548001, 102.3871387122750889 ) ) ;
#15249 = CARTESIAN_POINT ( 'NONE',  ( 231.2217848218749339, -31.41562499938547859, 102.3871387122750889 ) ) ;
#15250 = VERTEX_POINT ( 'NONE', #15991 ) ;
#15251 =( LENGTH_UNIT ( ) NAMED_UNIT ( * ) SI_UNIT ( .MILLI., .METRE. ) );
#15252 = CARTESIAN_POINT ( 'NONE',  ( -85.15643035625001289, -33.74062499938548854, -99.99999999999998579 ) ) ;
#15253 = CARTESIAN_POINT ( 'NONE',  ( 25.15499999999999758, 0.000000000000000000, 2.500000000000000444 ) ) ;
#15254 = EDGE_LOOP ( 'NONE', ( #10727, #14089, #6690 ) ) ;
#15255 = DIRECTION ( 'NONE',  ( 0.000000000000000000, -1.000000000000000000, 0.000000000000000000 ) ) ;
#15256 = CARTESIAN_POINT ( 'NONE',  ( 229.7064227204516556, -35.00000000000002132, -49.68450386720867584 ) ) ;
#15257 = CARTESIAN_POINT ( 'NONE',  ( -94.79999999999999716, -29.80000000000000426, -150.0000000000000000 ) ) ;
#15258 = ORIENTED_EDGE ( 'NONE', *, *, #16770, .F. ) ;
#15259 = ORIENTED_EDGE ( 'NONE', *, *, #4094, .T. ) ;
#15260 = CARTESIAN_POINT ( 'NONE',  ( -83.52979456739217312, -32.00000000000000000, 102.5803447510192257 ) ) ;
#15261 = CARTESIAN_POINT ( 'NONE',  ( 79.39999999999999147, -30.67500000000000071, -99.99999999999998579 ) ) ;
#15262 = CARTESIAN_POINT ( 'NONE',  ( -79.39999999999999147, -33.73124999877096997, 98.26794919243110371 ) ) ;
#15263 = EDGE_CURVE ( 'NONE', #18099, #10812, #9083, .T. ) ;
#15264 = CARTESIAN_POINT ( 'NONE',  ( -81.45486068924901701, -32.00000000000002132, -97.24663084804292623 ) ) ;
#15265 = CARTESIAN_POINT ( 'NONE',  ( 232.5999999999999375, -33.85312499938547859, 96.81714838363319586 ) ) ;
#15266 = CARTESIAN_POINT ( 'NONE',  ( 83.77821517812500929, -33.32812499938548711, -102.3871387122750889 ) ) ;
#15267 = CARTESIAN_POINT ( 'NONE',  ( 79.39999999999999147, -33.37500000000000000, -99.99999999999998579 ) ) ;
#15268 = CARTESIAN_POINT ( 'NONE',  ( 79.64356964374999848, -33.06562499938548427, -99.99999999999998579 ) ) ;
#15269 = ORIENTED_EDGE ( 'NONE', *, *, #11638, .T. ) ;
#15270 =( BOUNDED_CURVE ( )  B_SPLINE_CURVE ( 2, ( #16230, #5771, #14843, #7326, #4204, #16322, #4110, #10073, #19254 ),
 .UNSPECIFIED., .F., .F. ) 
 B_SPLINE_CURVE_WITH_KNOTS ( ( 3, 2, 2, 2, 3 ),
 ( 0.7708333333333332593, 0.7777777777777777901, 0.7916666666666666297, 0.8055555555555555802, 0.8125000000000000000 ),
 .UNSPECIFIED. ) 
 CURVE ( )  GEOMETRIC_REPRESENTATION_ITEM ( )  RATIONAL_B_SPLINE_CURVE ( ( 0.9330127018922192983, 0.9330127018922187432, 1.000000000000000000, 0.8660254037844387076, 1.000000000000000000, 0.8660254037844387076, 1.000000000000000000, 0.9330127018922194093, 0.9330127018922194093 ) ) 
 REPRESENTATION_ITEM ( '' )  );
#15271 = CARTESIAN_POINT ( 'NONE',  ( 235.5999999999999375, -32.92499999999999716, -50.00000000000011369 ) ) ;
#15272 = CARTESIAN_POINT ( 'NONE',  ( -79.39999999999999147, -34.76250000000000284, 101.7320508075688537 ) ) ;
#15273 = CARTESIAN_POINT ( 'NONE',  ( -83.90000000000000568, -30.97500000000000142, 97.40192378864668399 ) ) ;
#15274 = UNCERTAINTY_MEASURE_WITH_UNIT (LENGTH_MEASURE( 1.000000000000000082E-05 ), #16243, 'distance_accuracy_value', 'NONE');
#15275 = CARTESIAN_POINT ( 'NONE',  ( 230.5523683116323355, -32.00000000000000000, 101.8452947671440540 ) ) ;
#15276 = CARTESIAN_POINT ( 'NONE',  ( -85.15643035625001289, -31.15312499938548996, 99.99999999999998579 ) ) ;
#15277 = CARTESIAN_POINT ( 'NONE',  ( 231.2217848218749339, -34.37812499938547717, -52.38713871227520968 ) ) ;
#15278 = CARTESIAN_POINT ( 'NONE',  ( -79.39999999999999147, -30.18750000000000355, 98.26794919243110371 ) ) ;
#15279 = EDGE_LOOP ( 'NONE', ( #1569, #4687, #17765, #15424 ) ) ;
#15280 = CARTESIAN_POINT ( 'NONE',  ( -85.11710442811005350, -34.99993311519780548, 101.3183887536204537 ) ) ;
#15281 = CARTESIAN_POINT ( 'NONE',  ( 231.2217848218749339, -34.26562499938548001, 97.61286128772489690 ) ) ;
#15282 = DIRECTION ( 'NONE',  ( 1.000000000000000000, 0.000000000000000000, 0.000000000000000000 ) ) ;
#15283 = CARTESIAN_POINT ( 'NONE',  ( 229.9620029755564588, -32.00000000000001421, -50.81878454495714692 ) ) ;
#15284 = CARTESIAN_POINT ( 'NONE',  ( -79.64356964374998427, -32.24062499938548854, 98.40857419181659793 ) ) ;
#15285 = DIRECTION ( 'NONE',  ( 0.000000000000000000, 1.000000000000000000, 0.000000000000000000 ) ) ;
#15286 = CARTESIAN_POINT ( 'NONE',  ( 81.02178482187500208, -34.60312499938549280, 97.61286128772489690 ) ) ;
#15287 = CARTESIAN_POINT ( 'NONE',  ( 82.39999999999999147, -31.71562499938548640, -96.81714838363319586 ) ) ;
#15288 = CARTESIAN_POINT ( 'NONE',  ( 235.5999999999999943, -32.88749999999999574, -51.73205080756900287 ) ) ;
#15289 = CARTESIAN_POINT ( 'NONE',  ( -83.77821517812500929, -34.67812499938548854, 102.3871387122750889 ) ) ;
#15290 = CARTESIAN_POINT ( 'NONE',  ( -83.77821517812500929, -33.92812499938548854, -102.3871387122750889 ) ) ;
#15291 = PRODUCT_DEFINITION_CONTEXT ( 'detailed design', #18573, 'design' ) ;
#15292 = ORIENTED_EDGE ( 'NONE', *, *, #4624, .F. ) ;
#15293 = CARTESIAN_POINT ( 'NONE',  ( 79.64356964375001269, -33.21562499938548996, 98.40857419181659793 ) ) ;
#15294 = CARTESIAN_POINT ( 'NONE',  ( -85.40000000000000568, -33.13124999877096855, 98.26794919243111792 ) ) ;
#15295 = CARTESIAN_POINT ( 'NONE',  ( 82.40000000000000568, -30.00000000000000355, -99.99999999999998579 ) ) ;
#15296 = CARTESIAN_POINT ( 'NONE',  ( -83.77821517812500929, -33.32812499938548711, 102.3871387122750889 ) ) ;
#15297 =( BOUNDED_CURVE ( )  B_SPLINE_CURVE ( 2, ( #12810, #5401, #8126, #11344, #8410, #12613, #18586 ),
 .UNSPECIFIED., .F., .F. ) 
 B_SPLINE_CURVE_WITH_KNOTS ( ( 3, 2, 2, 3 ),
 ( 0.3702305174533203069, 0.3750000000000000000, 0.3888888888888888951, 0.3958333333333334259 ),
 .UNSPECIFIED. ) 
 CURVE ( )  GEOMETRIC_REPRESENTATION_ITEM ( )  RATIONAL_B_SPLINE_CURVE ( ( 0.9395835397642939846, 0.9539927561189023297, 1.000000000000000000, 0.8660254037844387076, 1.000000000000000000, 0.9330127018922185211, 0.9330127018922192983 ) ) 
 REPRESENTATION_ITEM ( '' )  );
#15298 = DIRECTION ( 'NONE',  ( 0.000000000000000000, 0.000000000000000000, -1.000000000000000000 ) ) ;
#15299 = ORIENTED_EDGE ( 'NONE', *, *, #10593, .T. ) ;
#15300 = CARTESIAN_POINT ( 'NONE',  ( -85.40000000000000568, -31.38749999999999574, -101.7320508075688679 ) ) ;
#15301 = CARTESIAN_POINT ( 'NONE',  ( 4.175813232069148562, -2.061359961916374495, -3.570380186727398097 ) ) ;
#15302 = DIRECTION ( 'NONE',  ( -0.000000000000000000, -1.000000000000000000, -0.000000000000000000 ) ) ;
#15303 = CARTESIAN_POINT ( 'NONE',  ( 82.40000000000000568, -30.00000000000000355, -99.99999999999998579 ) ) ;
#15304 = CARTESIAN_POINT ( 'NONE',  ( 232.5999999999999375, -32.98124999877095576, -47.00000000000011369 ) ) ;
#15305 = CARTESIAN_POINT ( 'NONE',  ( 235.3564303562499447, -34.04062499938547859, 98.40857419181659793 ) ) ;
#15306 = CARTESIAN_POINT ( 'NONE',  ( -79.39999999999999147, -33.32268749875867542, 99.99999999999998579 ) ) ;
#15307 = VERTEX_POINT ( 'NONE', #962 ) ;
#15308 = CARTESIAN_POINT ( 'NONE',  ( 232.5999999999999375, -33.26249999999999574, -53.00000000000011369 ) ) ;
#15309 = CARTESIAN_POINT ( 'NONE',  ( 82.40000000000000568, -34.38749999999999574, -102.9999999999999858 ) ) ;
#15310 = CARTESIAN_POINT ( 'NONE',  ( 229.8787539177868098, -32.00000000000000000, 99.52644304241978546 ) ) ;
#15311 = DIRECTION ( 'NONE',  ( -1.000000000000000000, 0.000000000000000000, 0.000000000000000000 ) ) ;
#15312 = CARTESIAN_POINT ( 'NONE',  ( 94.79999999999995453, -5.200000000000000178, 150.0000000000000000 ) ) ;
#15313 = CARTESIAN_POINT ( 'NONE',  ( 82.39999999999999147, -30.81562499938548427, -96.81714838363319586 ) ) ;
#15314 = CARTESIAN_POINT ( 'NONE',  ( -82.39999999999999147, -32.36250000000000426, 96.99999999999998579 ) ) ;
#15315 = EDGE_LOOP ( 'NONE', ( #9663, #5104, #18306, #9386 ) ) ;
#15316 = CARTESIAN_POINT ( 'NONE',  ( 235.3564303562499447, -32.69062499938547717, -51.59142580818350154 ) ) ;
#15317 = CARTESIAN_POINT ( 'NONE',  ( 0.000000000000000000, 0.000000000000000000, 0.000000000000000000 ) ) ;
#15318 = CARTESIAN_POINT ( 'NONE',  ( 229.8435696437499871, -32.54062499938547859, 98.40857419181659793 ) ) ;
#15319 = CARTESIAN_POINT ( 'NONE',  ( 232.5999999999999375, -30.36562499938548498, -53.18285161636690361 ) ) ;
#15320 = ADVANCED_FACE ( 'NONE', ( #2310 ), #17270, .F. ) ;
#15321 = DIRECTION ( 'NONE',  ( 1.387778780781445676E-15, 1.000000000000000000, 0.000000000000000000 ) ) ;
#15322 = EDGE_LOOP ( 'NONE', ( #1767, #8831, #12436 ) ) ;
#15323 = EDGE_LOOP ( 'NONE', ( #6343, #10845, #1811, #904 ) ) ;
#15324 = CARTESIAN_POINT ( 'NONE',  ( -79.68063642056705476, -32.00000000000000711, 98.73478688818576643 ) ) ;
#15325 = CARTESIAN_POINT ( 'NONE',  ( -80.90000000000000568, -33.84374999877096712, -97.40192378864668399 ) ) ;
#15326 = CARTESIAN_POINT ( 'NONE',  ( 82.40000000000000568, -30.00000000000000355, -96.99999999999998579 ) ) ;
#15327 = VERTEX_POINT ( 'NONE', #4073 ) ;
#15328 = DIRECTION ( 'NONE',  ( 1.000000000000000000, -1.387778780781445676E-15, -2.407412430484046130E-31 ) ) ;
#15329 = CARTESIAN_POINT ( 'NONE',  ( -80.90000000000000568, -34.59374999877096712, -102.5980762113533018 ) ) ;
#15330 = CARTESIAN_POINT ( 'NONE',  ( -80.90000000000000568, -31.94999999999999929, 97.40192378864668399 ) ) ;
#15331 = CARTESIAN_POINT ( 'NONE',  ( -83.90000000000000568, -31.36874999877096926, 97.40192378864668399 ) ) ;
#15332 = CARTESIAN_POINT ( 'NONE',  ( -79.39999999999999147, -33.31874999877096855, 99.99999999999998579 ) ) ;
#15333 = DIRECTION ( 'NONE',  ( -4.625929269271485791E-17, -1.000000000000000000, 0.000000000000000000 ) ) ;
#15334 =( BOUNDED_CURVE ( )  B_SPLINE_CURVE ( 2, ( #5064, #14038, #1736, #7887, #4974, #16881, #18158, #15509, #15217 ),
 .UNSPECIFIED., .F., .F. ) 
 B_SPLINE_CURVE_WITH_KNOTS ( ( 3, 2, 2, 2, 3 ),
 ( 0.7291666666666666297, 0.7361111111111111605, 0.7500000000000000000, 0.7638888888888888395, 0.7708333333333331483 ),
 .UNSPECIFIED. ) 
 CURVE ( )  GEOMETRIC_REPRESENTATION_ITEM ( )  RATIONAL_B_SPLINE_CURVE ( ( 0.9330127018922192983, 0.9330127018922187432, 1.000000000000000000, 0.8660254037844387076, 1.000000000000000000, 0.8660254037844387076, 1.000000000000000000, 0.9330127018922209636, 0.9330127018922194093 ) ) 
 REPRESENTATION_ITEM ( '' )  );
#15335 = EDGE_CURVE ( 'NONE', #18607, #15232, #14224, .T. ) ;
#15336 = CARTESIAN_POINT ( 'NONE',  ( 234.0999999999999375, -32.49374999877096570, 102.5980762113533018 ) ) ;
#15337 = SURFACE_STYLE_FILL_AREA ( #6269 ) ;
#15338 = CARTESIAN_POINT ( 'NONE',  ( 3.880206590543030742, 2.665671387532557279, 2.382921720510984276 ) ) ;
#15339 = CARTESIAN_POINT ( 'NONE',  ( 230.4884450829329694, -35.14114833091483803, 98.22820877610629964 ) ) ;
#15340 = EDGE_CURVE ( 'NONE', #138, #12892, #16082, .T. ) ;
#15341 = ORIENTED_EDGE ( 'NONE', *, *, #70, .T. ) ;
#15342 = SURFACE_STYLE_FILL_AREA ( #327 ) ;
#15343 = CARTESIAN_POINT ( 'NONE',  ( -83.77821517812500929, -35.01562499938548711, -97.61286128772489690 ) ) ;
#15344 = CARTESIAN_POINT ( 'NONE',  ( -2.500000000000000888, 0.000000000000000000, -4.974599999999998801 ) ) ;
#15345 = VERTEX_POINT ( 'NONE', #8460 ) ;
#15346 = CYLINDRICAL_SURFACE ( 'NONE', #18951, 7.500000000000020428 ) ;
#15347 = DIRECTION ( 'NONE',  ( -0.000000000000000000, -0.000000000000000000, -1.000000000000000000 ) ) ;
#15348 = CARTESIAN_POINT ( 'NONE',  ( 80.90000000000000568, -33.45000000000000284, 97.40192378864668399 ) ) ;
#15349 = VERTEX_POINT ( 'NONE', #5551 ) ;
#15350 = FACE_OUTER_BOUND ( 'NONE', #4329, .T. ) ;
#15351 = AXIS2_PLACEMENT_3D ( 'NONE', #6546, #3503, #9462 ) ;
#15352 = EDGE_LOOP ( 'NONE', ( #12806, #13105, #9480, #670 ) ) ;
#15353 = ORIENTED_EDGE ( 'NONE', *, *, #10956, .T. ) ;
#15354 = CARTESIAN_POINT ( 'NONE',  ( -81.45486068924900280, -32.00000000000002132, 102.7533691519570311 ) ) ;
#15355 = EDGE_CURVE ( 'NONE', #17378, #10782, #14508, .T. ) ;
#15356 = CARTESIAN_POINT ( 'NONE',  ( 85.40000000000000568, -30.45000000000000284, -99.99999999999998579 ) ) ;
#15357 = DIRECTION ( 'NONE',  ( 0.000000000000000000, -1.000000000000000000, 0.000000000000000000 ) ) ;
#15358 = CARTESIAN_POINT ( 'NONE',  ( -84.69813954184694182, -35.39427337414329600, 98.07164457472185859 ) ) ;
#15359 = CARTESIAN_POINT ( 'NONE',  ( -94.79999999999999716, -29.80000000000000426, -150.0000000000000000 ) ) ;
#15360 = CARTESIAN_POINT ( 'NONE',  ( 229.5999999999999375, -33.11249999999999716, 101.7320508075688821 ) ) ;
#15361 = CARTESIAN_POINT ( 'NONE',  ( 85.15643035625001289, -32.91562499938548569, -101.5914258081833879 ) ) ;
#15362 = FACE_OUTER_BOUND ( 'NONE', #16202, .T. ) ;
#15363 = CARTESIAN_POINT ( 'NONE',  ( -81.02178482187500208, -33.44062499938548427, 97.61286128772489690 ) ) ;
#15364 = VECTOR ( 'NONE', #787, 1000.000000000000000 ) ;
#15365 = AXIS2_PLACEMENT_3D ( 'NONE', #17784, #11713, #8689 ) ;
#15366 = CARTESIAN_POINT ( 'NONE',  ( 85.15643035624999868, -32.87812499938549138, -98.40857419181659793 ) ) ;
#15367 = ORIENTED_EDGE ( 'NONE', *, *, #18843, .F. ) ;
#15368 = CARTESIAN_POINT ( 'NONE',  ( 235.5999999999999943, -32.06249999999999289, -48.26794919243124582 ) ) ;
#15369 = ADVANCED_FACE ( 'NONE', ( #10130 ), #11590, .F. ) ;
#15370 = CARTESIAN_POINT ( 'NONE',  ( -82.39999999999999147, -34.83749999999999858, 103.4641016151377499 ) ) ;
#15371 = DIRECTION ( 'NONE',  ( 0.000000000000000000, 0.000000000000000000, 1.000000000000000000 ) ) ;
#15372 = CARTESIAN_POINT ( 'NONE',  ( 232.5999999999999943, -33.06562499938547717, 96.81714838363319586 ) ) ;
#15373 = CARTESIAN_POINT ( 'NONE',  ( -79.64356964375001269, -30.44062499938548783, 98.40857419181659793 ) ) ;
#15374 = CARTESIAN_POINT ( 'NONE',  ( 229.8435696437499303, -33.40312499938547575, -50.00000000000011369 ) ) ;
#15375 = CARTESIAN_POINT ( 'NONE',  ( -85.40000000000000568, -32.66250000000000142, 101.7320508075688679 ) ) ;
#15376 = ORIENTED_EDGE ( 'NONE', *, *, #3904, .F. ) ;
#15377 = CARTESIAN_POINT ( 'NONE',  ( -84.93364891667351912, -34.99959809868389016, 98.35626849035328689 ) ) ;
#15378 = EDGE_CURVE ( 'NONE', #3413, #5719, #7287, .T. ) ;
#15379 = PRODUCT_RELATED_PRODUCT_CATEGORY ( 'part', '', ( #2493 ) ) ;
#15380 = CARTESIAN_POINT ( 'NONE',  ( -80.90000000000000568, -34.74374999877097281, 102.5980762113533018 ) ) ;
#15381 = CARTESIAN_POINT ( 'NONE',  ( 82.39999999999999147, -31.60312499938548569, 103.1828516163667899 ) ) ;
#15382 = CLOSED_SHELL ( 'NONE', ( #663, #18454, #11322, #18549, #4355, #9518, #6488, #7662, #7721, #4718, #8156, #8371, #10037, #15123, #10624, #16203, #2112, #17602, #19201, #18811, #4695, #4222, #12939, #12984, #16754, #5669, #6155, #2317, #3364, #5220, #4608, #10321 ) ) ;
#15383 = CARTESIAN_POINT ( 'NONE',  ( 85.40000000000000568, -32.68124999877097281, -98.26794919243111792 ) ) ;
#15384 =( BOUNDED_CURVE ( )  B_SPLINE_CURVE ( 2, ( #4560, #3181, #14915, #7676, #17950, #371, #6127, #6322, #10517 ),
 .UNSPECIFIED., .F., .F. ) 
 B_SPLINE_CURVE_WITH_KNOTS ( ( 3, 2, 2, 2, 3 ),
 ( 0.5625000000000000000, 0.5694444444444444198, 0.5833333333333333703, 0.5972222222222222099, 0.6041666666666666297 ),
 .UNSPECIFIED. ) 
 CURVE ( )  GEOMETRIC_REPRESENTATION_ITEM ( )  RATIONAL_B_SPLINE_CURVE ( ( 0.9330127018922194093, 0.9330127018922194093, 1.000000000000000000, 0.8660254037844387076, 1.000000000000000000, 0.8660254037844387076, 1.000000000000000000, 0.9330127018922198534, 0.9330127018922192983 ) ) 
 REPRESENTATION_ITEM ( '' )  );
#15385 = CARTESIAN_POINT ( 'NONE',  ( -82.39999999999999147, -31.71562499938548640, 96.81714838363319586 ) ) ;
#15386 = CARTESIAN_POINT ( 'NONE',  ( -85.15643035624999868, -32.02817623523066004, -98.94122380911285575 ) ) ;
#15387 = CARTESIAN_POINT ( 'NONE',  ( 81.02178482187500208, -35.05312499938548854, 97.61286128772489690 ) ) ;
#15388 = B_SPLINE_CURVE_WITH_KNOTS ( 'NONE', 3,
 ( #12889, #1072, #19046, #14730, #5670, #6849, #12983, #983, #18860, #7030, #18954, #5578, #4095, #11613, #17580, #4191 ),
 .UNSPECIFIED., .F., .F.,
 ( 4, 2, 2, 2, 2, 2, 2, 4 ),
 ( 0.000000000000000000, 0.0005391024520904045712, 0.001078204904180809142, 0.002156409808361649943, 0.002695512260452069802, 0.003234614712542490094, 0.003773717164632910820, 0.004312819616723331112 ),
 .UNSPECIFIED. ) ;
#15389 = CARTESIAN_POINT ( 'NONE',  ( 83.77821517812500929, -31.67812499938548498, -97.61286128772489690 ) ) ;
#15390 = DIRECTION ( 'NONE',  ( -1.000000000000000000, 0.000000000000000000, 0.000000000000000000 ) ) ;
#15391 = CARTESIAN_POINT ( 'NONE',  ( -83.77821517812500929, -33.47812499938548569, 97.61286128772489690 ) ) ;
#15392 = CARTESIAN_POINT ( 'NONE',  ( -81.02178482187500208, -33.70312499938548711, -97.61286128772489690 ) ) ;
#15393 =( BOUNDED_SURFACE ( )  B_SPLINE_SURFACE ( 1, 2, ( 
 ( #7025, #18662, #979, #12979, #2331, #6934, #5573, #10052, #10147, #16011, #8202, #6045, #1449, #14724, #19235, #3097, #16495, #8864, #12088, #10429, #16211, #4673, #6138, #10249, #14629, #8676, #2817, #7595, #8774, #10527, #17865, #4284, #5753, #13457, #1642, #11992, #92, #1360, #11894, #4381, #13548, #19136, #4476, #18062, #9057, #3003, #16393, #7304, #13261, #10622, #2716, #17960, #4570, #15022, #8959, #1264, #188, #7211, #14927, #13164, #1774, #11702, #13365, #17671, #2912, #5851, #11805, #17774, #10338, #1553, #7501, #7402, #16302, #14821, #5947, #3578, #18345, #12284, #9439, #9538, #15405, #570, #16588, #7688, #668, #13644, #4967, #12184, #6332, #1918, #3192, #3391, #10909, #285, #7787, #4774, #2015, #18534, #6236, #12566, #6525, #15305, #9246, #13741, #16967, #11000, #9342, #6617, #16875, #10717, #5150, #9151, #16681, #15114, #1730, #3287, #2119, #15210, #5058, #12379, #18152, #1827, #7975, #15504, #12471, #13931, #379, #6423, #18248, #4866, #10810, #13832, #18439, #16776, #474 ),
 ( #7881, #3479, #8079, #14032, #7170, #2663, #4047, #17726, #8530, #17528, #2770, #14480, #5620, #14678, #15606, #761, #11565, #13216, #17623, #18633, #11096, #19187, #4238, #1110, #17166, #6714, #1313, #2865, #16059, #16256, #11659, #13028, #8823, #8176, #1213, #1406, #5803, #10195, #13119, #11200, #10006, #19290, #7358, #8725, #7261, #4336, #19090, #13315, #11755, #17065, #16159, #3680, #8624, #9645, #14577, #14123, #4140, #10296, #14780, #15961, #2212, #12660, #5254, #10103, #2568, #5711, #7069, #18999, #7642, #1601, #18113, #18208, #4727, #9201, #5904, #16349, #9301, #2960, #13597, #1505, #14978, #10583, #11850, #12042, #238, #8914, #16446, #13414, #10670, #7839, #14875, #1880, #15164, #4630, #17917, #3056, #6290, #343, #18018, #15265, #6196, #44, #13793, #17818, #5995, #4428, #10388, #11947, #10766, #4524, #13703, #1691, #7456, #10482, #16640, #4826, #1782, #3243, #9018, #15071, #7548, #13507, #145, #3147, #7746, #6095, #9107, #12144, #12239, #16548, #16731, #3340, #5208, #14180, #3730 ) ),
 .UNSPECIFIED., .F., .F., .F. ) 
 B_SPLINE_SURFACE_WITH_KNOTS ( ( 2, 2 ),
 ( 3, 2, 2, 2, 2, 2, 2, 2, 2, 2, 2, 2, 2, 2, 2, 2, 2, 2, 2, 2, 2, 2, 2, 2, 2, 2, 2, 2, 2, 2, 2, 2, 2, 2, 2, 2, 2, 2, 2, 2, 2, 2, 2, 2, 2, 2, 2, 2, 2, 2, 2, 2, 2, 2, 2, 2, 2, 2, 2, 2, 2, 2, 2, 2, 2, 2, 2, 3 ),
 ( 0.000000000000000000, 1.000000000000000000 ),
 ( 0.000000000000000000, 0.01388888888888888812, 0.02777777777777777624, 0.04166666666666666435, 0.05555555555555555247, 0.06944444444444444753, 0.08333333333333332871, 0.09722222222222222376, 0.1111111111111111049, 0.1250000000000000000, 0.1388888888888888951, 0.1527777777777777901, 0.1666666666666666574, 0.1805555555555555525, 0.1944444444444444475, 0.2083333333333333426, 0.2222222222222222099, 0.2361111111111111049, 0.2500000000000000000, 0.2638888888888888951, 0.2777777777777777901, 0.2916666666666666852, 0.3055555555555555802, 0.3194444444444444198, 0.3333333333333333148, 0.3472222222222222099, 0.3611111111111111049, 0.3750000000000000000, 0.3888888888888888951, 0.4027777777777777901, 0.4166666666666666852, 0.4305555555555555802, 0.4444444444444444198, 0.4583333333333333148, 0.4722222222222222099, 0.4861111111111111049, 0.5000000000000000000, 0.5138888888888888395, 0.5277777777777777901, 0.5416666666666666297, 0.5555555555555555802, 0.5694444444444444198, 0.5833333333333333703, 0.5972222222222222099, 0.6111111111111111605, 0.6250000000000000000, 0.6388888888888888395, 0.6527777777777777901, 0.6666666666666666297, 0.6805555555555555802, 0.6944444444444444198, 0.7083333333333333703, 0.7222222222222222099, 0.7361111111111111605, 0.7500000000000000000, 0.7638888888888888395, 0.7777777777777777901, 0.7916666666666666297, 0.8055555555555555802, 0.8194444444444444198, 0.8333333333333333703, 0.8472222222222222099, 0.8611111111111111605, 0.8750000000000000000, 0.8888888888888888395, 0.9027777777777777901, 0.9166666666666666297, 0.9258785565094813652 ),
 .UNSPECIFIED. ) 
 GEOMETRIC_REPRESENTATION_ITEM ( )  RATIONAL_B_SPLINE_SURFACE ( (
 ( 1.000000000000000000, 0.8660254037844387076, 1.000000000000000000, 0.8660254037844387076, 1.000000000000000000, 0.8660254037844387076, 1.000000000000000000, 0.8660254037844387076, 1.000000000000000000, 0.8660254037844387076, 1.000000000000000000, 0.8660254037844387076, 1.000000000000000000, 0.8660254037844387076, 1.000000000000000000, 0.8660254037844387076, 1.000000000000000000, 0.8660254037844387076, 1.000000000000000000, 0.8660254037844387076, 1.000000000000000000, 0.8660254037844387076, 1.000000000000000000, 0.8660254037844387076, 1.000000000000000000, 0.8660254037844387076, 1.000000000000000000, 0.8660254037844387076, 1.000000000000000000, 0.8660254037844387076, 1.000000000000000000, 0.8660254037844387076, 1.000000000000000000, 0.8660254037844387076, 1.000000000000000000, 0.8660254037844387076, 1.000000000000000000, 0.8660254037844387076, 1.000000000000000000, 0.8660254037844387076, 1.000000000000000000, 0.8660254037844387076, 1.000000000000000000, 0.8660254037844387076, 1.000000000000000000, 0.8660254037844387076, 1.000000000000000000, 0.8660254037844387076, 1.000000000000000000, 0.8660254037844387076, 1.000000000000000000, 0.8660254037844387076, 1.000000000000000000, 0.8660254037844387076, 1.000000000000000000, 0.8660254037844387076, 1.000000000000000000, 0.8660254037844387076, 1.000000000000000000, 0.8660254037844387076, 1.000000000000000000, 0.8660254037844387076, 1.000000000000000000, 0.8660254037844387076, 1.000000000000000000, 0.8660254037844387076, 1.000000000000000000, 0.8660254037844387076, 1.000000000000000000, 0.8660254037844387076, 1.000000000000000000, 0.8660254037844387076, 1.000000000000000000, 0.8660254037844387076, 1.000000000000000000, 0.8660254037844387076, 1.000000000000000000, 0.8660254037844387076, 1.000000000000000000, 0.8660254037844387076, 1.000000000000000000, 0.8660254037844387076, 1.000000000000000000, 0.8660254037844387076, 1.000000000000000000, 0.8660254037844387076, 1.000000000000000000, 0.8660254037844387076, 1.000000000000000000, 0.8660254037844387076, 1.000000000000000000, 0.8660254037844387076, 1.000000000000000000, 0.8660254037844387076, 1.000000000000000000, 0.8660254037844387076, 1.000000000000000000, 0.8660254037844387076, 1.000000000000000000, 0.8660254037844387076, 1.000000000000000000, 0.8660254037844387076, 1.000000000000000000, 0.8660254037844387076, 1.000000000000000000, 0.8660254037844387076, 1.000000000000000000, 0.8660254037844387076, 1.000000000000000000, 0.8660254037844387076, 1.000000000000000000, 0.8660254037844387076, 1.000000000000000000, 0.8660254037844387076, 1.000000000000000000, 0.8660254037844387076, 1.000000000000000000, 0.8660254037844387076, 1.000000000000000000, 0.8660254037844387076, 1.000000000000000000, 0.8660254037844387076, 1.000000000000000000, 0.8660254037844387076, 1.000000000000000000, 0.8660254037844387076, 1.000000000000000000, 0.8660254037844387076, 1.000000000000000000, 0.8660254037844387076, 1.000000000000000000, 0.8660254037844387076, 1.000000000000000000, 0.9111405360107203144, 0.9401542295229963209),
 ( 1.000000000000000000, 0.8660254037844387076, 1.000000000000000000, 0.8660254037844387076, 1.000000000000000000, 0.8660254037844387076, 1.000000000000000000, 0.8660254037844387076, 1.000000000000000000, 0.8660254037844387076, 1.000000000000000000, 0.8660254037844387076, 1.000000000000000000, 0.8660254037844387076, 1.000000000000000000, 0.8660254037844387076, 1.000000000000000000, 0.8660254037844387076, 1.000000000000000000, 0.8660254037844387076, 1.000000000000000000, 0.8660254037844387076, 1.000000000000000000, 0.8660254037844387076, 1.000000000000000000, 0.8660254037844387076, 1.000000000000000000, 0.8660254037844387076, 1.000000000000000000, 0.8660254037844387076, 1.000000000000000000, 0.8660254037844387076, 1.000000000000000000, 0.8660254037844387076, 1.000000000000000000, 0.8660254037844387076, 1.000000000000000000, 0.8660254037844387076, 1.000000000000000000, 0.8660254037844387076, 1.000000000000000000, 0.8660254037844387076, 1.000000000000000000, 0.8660254037844387076, 1.000000000000000000, 0.8660254037844387076, 1.000000000000000000, 0.8660254037844387076, 1.000000000000000000, 0.8660254037844387076, 1.000000000000000000, 0.8660254037844387076, 1.000000000000000000, 0.8660254037844387076, 1.000000000000000000, 0.8660254037844387076, 1.000000000000000000, 0.8660254037844387076, 1.000000000000000000, 0.8660254037844387076, 1.000000000000000000, 0.8660254037844387076, 1.000000000000000000, 0.8660254037844387076, 1.000000000000000000, 0.8660254037844387076, 1.000000000000000000, 0.8660254037844387076, 1.000000000000000000, 0.8660254037844387076, 1.000000000000000000, 0.8660254037844387076, 1.000000000000000000, 0.8660254037844387076, 1.000000000000000000, 0.8660254037844387076, 1.000000000000000000, 0.8660254037844387076, 1.000000000000000000, 0.8660254037844387076, 1.000000000000000000, 0.8660254037844387076, 1.000000000000000000, 0.8660254037844387076, 1.000000000000000000, 0.8660254037844387076, 1.000000000000000000, 0.8660254037844387076, 1.000000000000000000, 0.8660254037844387076, 1.000000000000000000, 0.8660254037844387076, 1.000000000000000000, 0.8660254037844387076, 1.000000000000000000, 0.8660254037844387076, 1.000000000000000000, 0.8660254037844387076, 1.000000000000000000, 0.8660254037844387076, 1.000000000000000000, 0.8660254037844387076, 1.000000000000000000, 0.8660254037844387076, 1.000000000000000000, 0.8660254037844387076, 1.000000000000000000, 0.8660254037844387076, 1.000000000000000000, 0.8660254037844387076, 1.000000000000000000, 0.8660254037844387076, 1.000000000000000000, 0.8660254037844387076, 1.000000000000000000, 0.8660254037844387076, 1.000000000000000000, 0.8660254037844387076, 1.000000000000000000, 0.8660254037844387076, 1.000000000000000000, 0.8660254037844387076, 1.000000000000000000, 0.8660254037844387076, 1.000000000000000000, 0.8660254037844387076, 1.000000000000000000, 0.8660254037844387076, 1.000000000000000000, 0.8660254037844387076, 1.000000000000000000, 0.8660254037844387076, 1.000000000000000000, 0.9111405360107203144, 0.9401542295229963209) ) ) 
 REPRESENTATION_ITEM ( '' )  SURFACE ( )  );
#15394 = ORIENTED_EDGE ( 'NONE', *, *, #14987, .T. ) ;
#15395 = CARTESIAN_POINT ( 'NONE',  ( 85.15643035624999868, -33.89062499938548711, 101.5914258081833879 ) ) ;
#15396 = DIRECTION ( 'NONE',  ( 0.000000000000000000, 0.000000000000000000, -1.000000000000000000 ) ) ;
#15397 = CARTESIAN_POINT ( 'NONE',  ( -83.77821517812500929, -31.11562499938548498, 97.61286128772489690 ) ) ;
#15398 = CARTESIAN_POINT ( 'NONE',  ( -81.02178482187500208, -34.00312499938548427, 97.61286128772489690 ) ) ;
#15399 = CARTESIAN_POINT ( 'NONE',  ( 85.40000000000000568, -33.13124999877096855, 101.7320508075688821 ) ) ;
#15400 = EDGE_LOOP ( 'NONE', ( #1703, #13582, #468, #17593 ) ) ;
#15401 = CARTESIAN_POINT ( 'NONE',  ( -79.39999999999999147, -34.68750000000000000, -101.7320508075688821 ) ) ;
#15402 = CARTESIAN_POINT ( 'NONE',  ( 246.9999999999999716, -35.00000000000000000, 150.0000000000000000 ) ) ;
#15403 = DIRECTION ( 'NONE',  ( 0.000000000000000000, 0.000000000000000000, 1.000000000000000000 ) ) ;
#15404 = CARTESIAN_POINT ( 'NONE',  ( -85.15643035625001289, -34.75312499938548427, -99.99999999999998579 ) ) ;
#15405 = CARTESIAN_POINT ( 'NONE',  ( 233.9782151781249411, -33.25312499938547717, 102.3871387122750889 ) ) ;
#15406 = CARTESIAN_POINT ( 'NONE',  ( -79.39999999999999147, -34.26018749875867542, 101.7320508075688537 ) ) ;
#15407 = VERTEX_POINT ( 'NONE', #11782 ) ;
#15408 = FACE_OUTER_BOUND ( 'NONE', #15236, .T. ) ;
#15409 = CARTESIAN_POINT ( 'NONE',  ( 82.39999999999999147, -32.98124999877096286, -102.9999999999999858 ) ) ;
#15410 = CARTESIAN_POINT ( 'NONE',  ( 111.5000000000000142, 12.69999999999998508, 30.20101012677667285 ) ) ;
#15411 = CARTESIAN_POINT ( 'NONE',  ( 113.0000000000000142, 15.19999999999997442, -145.0000000000000000 ) ) ;
#15412 = DIRECTION ( 'NONE',  ( -0.000000000000000000, -1.000000000000000000, -0.000000000000000000 ) ) ;
#15413 = CARTESIAN_POINT ( 'NONE',  ( 82.39999999999999147, -32.39062499938548001, -103.1828516163667899 ) ) ;
#15414 = CARTESIAN_POINT ( 'NONE',  ( 4.093692494532766624, 2.021783646005775203, 3.501831996793853818 ) ) ;
#15415 =( BOUNDED_SURFACE ( )  B_SPLINE_SURFACE ( 3, 2, ( 
 ( #4966, #18804, #15675 ),
 ( #9150, #12183, #3843 ),
 ( #12283, #2284, #15113 ),
 ( #7686, #15771, #10809 ),
 ( #284, #11176, #13643 ),
 ( #17142, #2380, #8248 ) ),
 .UNSPECIFIED., .F., .F., .F. ) 
 B_SPLINE_SURFACE_WITH_KNOTS ( ( 4, 2, 4 ),
 ( 3, 3 ),
 ( 0.02032853247518126918, 0.02278863295364821906, 0.02524873343211516893 ),
 ( 0.000000000000000000, 1.000000000000000000 ),
 .UNSPECIFIED. ) 
 GEOMETRIC_REPRESENTATION_ITEM ( )  RATIONAL_B_SPLINE_SURFACE ( (
 ( 1.000000000000000000, 0.8047781615896838492, 1.000000000000000000),
 ( 1.000000000000000000, 0.8123767586288186404, 1.000000000000000000),
 ( 1.000000000000000000, 0.8190662415565814758, 1.000000000000000000),
 ( 1.000000000000000000, 0.8192361015667604107, 1.000000000000000000),
 ( 1.000000000000000000, 0.8126135807104967190, 1.000000000000000000),
 ( 1.000000000000000000, 0.8047712338318580017, 1.000000000000000000) ) ) 
 REPRESENTATION_ITEM ( '' )  SURFACE ( )  );
#15416 = ORIENTED_EDGE ( 'NONE', *, *, #11528, .T. ) ;
#15417 = CARTESIAN_POINT ( 'NONE',  ( 83.90000000000000568, -30.76874999877097139, 97.40192378864668399 ) ) ;
#15418 = PRODUCT_CONTEXT ( 'NONE', #7067, 'mechanical' ) ;
#15419 = CARTESIAN_POINT ( 'NONE',  ( 229.8435696437499303, -32.05312499938548143, 99.99999999999998579 ) ) ;
#15420 = CARTESIAN_POINT ( 'NONE',  ( 232.5999999999999375, -35.23124999877096286, -46.53589838486234953 ) ) ;
#15421 = CARTESIAN_POINT ( 'NONE',  ( -82.39999999999999147, -32.72812499938548569, 103.1828516163667899 ) ) ;
#15422 = CARTESIAN_POINT ( 'NONE',  ( 4.071447262713888016, 4.041451884327382338, 0.000000000000000000 ) ) ;
#15423 = ORIENTED_EDGE ( 'NONE', *, *, #17238, .T. ) ;
#15424 = ORIENTED_EDGE ( 'NONE', *, *, #18568, .F. ) ;
#15425 = CARTESIAN_POINT ( 'NONE',  ( 4.175572532730930320, 2.061029303918049393, -3.569807470274390937 ) ) ;
#15426 = CARTESIAN_POINT ( 'NONE',  ( -82.40000000000001990, -32.13750000000000284, -97.00000000000000000 ) ) ;
#15427 = FACE_OUTER_BOUND ( 'NONE', #975, .T. ) ;
#15428 = ORIENTED_EDGE ( 'NONE', *, *, #6731, .T. ) ;
#15429 = CARTESIAN_POINT ( 'NONE',  ( 79.64356964374999848, -32.27812499938548996, 99.99999999999998579 ) ) ;
#15430 = CARTESIAN_POINT ( 'NONE',  ( -85.40000000000000568, -34.89374999877097139, -99.99999999999998579 ) ) ;
#15431 = DIRECTION ( 'NONE',  ( 0.000000000000000000, 1.000000000000000000, 0.000000000000000000 ) ) ;
#15432 = CARTESIAN_POINT ( 'NONE',  ( -85.40000000000000568, -32.68124999877097281, 98.26794919243111792 ) ) ;
#15433 = CARTESIAN_POINT ( 'NONE',  ( -83.90000000000000568, -34.96874999877096712, 97.40192378864668399 ) ) ;
#15434 = CARTESIAN_POINT ( 'NONE',  ( -82.40000000000000568, -50.00000000000000000, 107.5000000000000142 ) ) ;
#15435 = EDGE_CURVE ( 'NONE', #5530, #7316, #1250, .T. ) ;
#15436 = ADVANCED_FACE ( 'NONE', ( #14803 ), #17756, .F. ) ;
#15437 = CARTESIAN_POINT ( 'NONE',  ( 79.39999999999999147, -34.18124999877097281, -98.26794919243110371 ) ) ;
#15438 = CARTESIAN_POINT ( 'NONE',  ( 232.6092389720418510, -31.99999999999999289, 102.8695224571928719 ) ) ;
#15439 = CARTESIAN_POINT ( 'NONE',  ( 232.5999999999999375, -34.75312499938547717, 96.81714838363319586 ) ) ;
#15440 = VERTEX_POINT ( 'NONE', #11876 ) ;
#15441 = CARTESIAN_POINT ( 'NONE',  ( -79.64356964375001269, -34.90312499938548285, -98.40857419181659793 ) ) ;
#15442 = CARTESIAN_POINT ( 'NONE',  ( 4.151274195509469855, 4.079825909417643004, -6.022632805413305277E-17 ) ) ;
#15443 = ORIENTED_EDGE ( 'NONE', *, *, #3496, .F. ) ;
#15444 = PLANE ( 'NONE',  #12705 ) ;
#15445 = CARTESIAN_POINT ( 'NONE',  ( 82.39999999999999147, -33.48750000000000426, 97.00000000000000000 ) ) ;
#15446 = UNCERTAINTY_MEASURE_WITH_UNIT (LENGTH_MEASURE( 1.000000000000000082E-05 ), #7533, 'distance_accuracy_value', 'NONE');
#15447 = CARTESIAN_POINT ( 'NONE',  ( 3.680118525130245732, -2.494084732383344605, -0.3507732604232533524 ) ) ;
#15448 = ORIENTED_EDGE ( 'NONE', *, *, #15167, .F. ) ;
#15449 = DIRECTION ( 'NONE',  ( -0.000000000000000000, -0.000000000000000000, -1.000000000000000000 ) ) ;
#15450 = EDGE_CURVE ( 'NONE', #16850, #13270, #3234, .T. ) ;
#15451 = CIRCLE ( 'NONE', #9859, 2.199999999999993516 ) ;
#15453 = ADVANCED_FACE ( 'NONE', ( #5831 ), #16281, .F. ) ;
#15452 = VERTEX_POINT ( 'NONE', #16572 ) ;
#15454 = ORIENTED_EDGE ( 'NONE', *, *, #13559, .T. ) ;
#15455 = CARTESIAN_POINT ( 'NONE',  ( -79.93183330737464587, -32.00000000000002132, 101.6855250459192206 ) ) ;
#15456 = CARTESIAN_POINT ( 'NONE',  ( 85.40000000000000568, -31.31250000000000000, -101.7320508075688679 ) ) ;
#15457 = DIRECTION ( 'NONE',  ( -0.000000000000000000, -1.000000000000000000, -0.000000000000000000 ) ) ;
#15458 = EDGE_CURVE ( 'NONE', #10188, #1970, #3173, .T. ) ;
#15459 =( BOUNDED_SURFACE ( )  B_SPLINE_SURFACE ( 1, 2, ( 
 ( #12957, #5261, #15611, #17461, #12865, #4072, #10032, #2595, #2309, #11207, #8273, #8555, #14223, #861, #5156, #11102, #17070, #2406, #14128, #9651, #8181, #18836, #6824, #766, #6719, #12664, #18739, #17268, #9837, #11301, #15801, #19115, #7482, #11781, #19317, #15004, #13438, #8650, #17841, #14802, #10320, #1532, #1429, #7382, #4455, #4550, #17755, #11684, #13342, #5928, #11874, #4360, #4264, #19022, #5735, #1622, #10223, #16280, #10410, #16374, #19213, #17554, #69, #10507, #2982, #8938, #2693, #17651, #13056, #13240, #6022, #16189, #5830, #2797, #11971, #14904, #17939, #3079, #5643, #8750, #11589, #14702, #2890, #16474, #9039, #8846, #4170, #10129, #16087, #14609, #1240, #7192, #1339, #13141, #7286, #549, #6219, #7769, #264, #13911, #12358, #7957, #16950, #4655, #10791, #7863, #13814, #1711, #18419, #12166, #3461, #18133, #18230, #4753, #6507, #10697, #15286, #4944, #6405, #15096, #15485, #1901, #9223, #16857, #166, #6311, #13528, #9420, #15387, #456, #16663, #13622, #3267, #15188, #1805 ),
 ( #2000, #12452, #18327, #5039, #7666, #7575, #3562, #10889, #10981, #9521, #6117, #12069, #18044, #10605, #16571, #3172, #9132, #13722, #363, #12265, #4846, #16753, #3370, #9322, #15682, #17339, #5134, #3848, #18517, #8252, #9814, #8439, #6698, #12642, #742, #15877, #2098, #6801, #18810, #8154, #11079, #11182, #5234, #14391, #17244, #18616, #1030, #14013, #2384, #9718, #17048, #8346, #17146, #649, #6982, #3660, #6892, #3949, #15586, #11473, #2196, #9625, #3752, #2288, #15776, #5435, #14106, #937, #9914, #14301, #2481, #14202, #839, #11372, #12842, #12934, #18904, #5525, #12748, #18715, #5338, #17440, #11275, #4051, #10010, #8058, #6598, #12546, #11569, #17820, #13032, #10299, #11664, #46, #4430, #5623, #2962, #14682, #1316, #17627, #14582, #2667, #10390, #7265, #2867, #17919, #16351, #17532, #1408, #17730, #13219, #8917, #4339, #16259, #7361, #7458, #19192, #1217, #8826, #14782, #13317, #5807, #7173, #2573, #8628, #4527, #13123, #11758, #19293, #5906, #2773, #1116, #14879, #13416, #11852 ) ),
 .UNSPECIFIED., .F., .F., .F. ) 
 B_SPLINE_SURFACE_WITH_KNOTS ( ( 2, 2 ),
 ( 3, 2, 2, 2, 2, 2, 2, 2, 2, 2, 2, 2, 2, 2, 2, 2, 2, 2, 2, 2, 2, 2, 2, 2, 2, 2, 2, 2, 2, 2, 2, 2, 2, 2, 2, 2, 2, 2, 2, 2, 2, 2, 2, 2, 2, 2, 2, 2, 2, 2, 2, 2, 2, 2, 2, 2, 2, 2, 2, 2, 2, 2, 2, 2, 2, 2, 2, 3 ),
 ( 0.000000000000000000, 1.000000000000000000 ),
 ( 0.000000000000000000, 0.01388888888888888812, 0.02777777777777777624, 0.04166666666666666435, 0.05555555555555555247, 0.06944444444444444753, 0.08333333333333332871, 0.09722222222222222376, 0.1111111111111111049, 0.1250000000000000000, 0.1388888888888888951, 0.1527777777777777901, 0.1666666666666666574, 0.1805555555555555525, 0.1944444444444444475, 0.2083333333333333426, 0.2222222222222222099, 0.2361111111111111049, 0.2500000000000000000, 0.2638888888888888951, 0.2777777777777777901, 0.2916666666666666852, 0.3055555555555555802, 0.3194444444444444198, 0.3333333333333333148, 0.3472222222222222099, 0.3611111111111111049, 0.3750000000000000000, 0.3888888888888888951, 0.4027777777777777901, 0.4166666666666666852, 0.4305555555555555802, 0.4444444444444444198, 0.4583333333333333148, 0.4722222222222222099, 0.4861111111111111049, 0.5000000000000000000, 0.5138888888888888395, 0.5277777777777777901, 0.5416666666666666297, 0.5555555555555555802, 0.5694444444444444198, 0.5833333333333333703, 0.5972222222222222099, 0.6111111111111111605, 0.6250000000000000000, 0.6388888888888888395, 0.6527777777777777901, 0.6666666666666666297, 0.6805555555555555802, 0.6944444444444444198, 0.7083333333333333703, 0.7222222222222222099, 0.7361111111111111605, 0.7500000000000000000, 0.7638888888888888395, 0.7777777777777777901, 0.7916666666666666297, 0.8055555555555555802, 0.8194444444444444198, 0.8333333333333333703, 0.8472222222222222099, 0.8611111111111111605, 0.8750000000000000000, 0.8888888888888888395, 0.9027777777777777901, 0.9166666666666666297, 0.9258785565094813652 ),
 .UNSPECIFIED. ) 
 GEOMETRIC_REPRESENTATION_ITEM ( )  RATIONAL_B_SPLINE_SURFACE ( (
 ( 1.000000000000000000, 0.8660254037844387076, 1.000000000000000000, 0.8660254037844387076, 1.000000000000000000, 0.8660254037844387076, 1.000000000000000000, 0.8660254037844387076, 1.000000000000000000, 0.8660254037844387076, 1.000000000000000000, 0.8660254037844387076, 1.000000000000000000, 0.8660254037844387076, 1.000000000000000000, 0.8660254037844387076, 1.000000000000000000, 0.8660254037844387076, 1.000000000000000000, 0.8660254037844387076, 1.000000000000000000, 0.8660254037844387076, 1.000000000000000000, 0.8660254037844387076, 1.000000000000000000, 0.8660254037844387076, 1.000000000000000000, 0.8660254037844387076, 1.000000000000000000, 0.8660254037844387076, 1.000000000000000000, 0.8660254037844387076, 1.000000000000000000, 0.8660254037844387076, 1.000000000000000000, 0.8660254037844387076, 1.000000000000000000, 0.8660254037844387076, 1.000000000000000000, 0.8660254037844387076, 1.000000000000000000, 0.8660254037844387076, 1.000000000000000000, 0.8660254037844387076, 1.000000000000000000, 0.8660254037844387076, 1.000000000000000000, 0.8660254037844387076, 1.000000000000000000, 0.8660254037844387076, 1.000000000000000000, 0.8660254037844387076, 1.000000000000000000, 0.8660254037844387076, 1.000000000000000000, 0.8660254037844387076, 1.000000000000000000, 0.8660254037844387076, 1.000000000000000000, 0.8660254037844387076, 1.000000000000000000, 0.8660254037844387076, 1.000000000000000000, 0.8660254037844387076, 1.000000000000000000, 0.8660254037844387076, 1.000000000000000000, 0.8660254037844387076, 1.000000000000000000, 0.8660254037844387076, 1.000000000000000000, 0.8660254037844387076, 1.000000000000000000, 0.8660254037844387076, 1.000000000000000000, 0.8660254037844387076, 1.000000000000000000, 0.8660254037844387076, 1.000000000000000000, 0.8660254037844387076, 1.000000000000000000, 0.8660254037844387076, 1.000000000000000000, 0.8660254037844387076, 1.000000000000000000, 0.8660254037844387076, 1.000000000000000000, 0.8660254037844387076, 1.000000000000000000, 0.8660254037844387076, 1.000000000000000000, 0.8660254037844387076, 1.000000000000000000, 0.8660254037844387076, 1.000000000000000000, 0.8660254037844387076, 1.000000000000000000, 0.8660254037844387076, 1.000000000000000000, 0.8660254037844387076, 1.000000000000000000, 0.8660254037844387076, 1.000000000000000000, 0.8660254037844387076, 1.000000000000000000, 0.8660254037844387076, 1.000000000000000000, 0.8660254037844387076, 1.000000000000000000, 0.8660254037844387076, 1.000000000000000000, 0.8660254037844387076, 1.000000000000000000, 0.8660254037844387076, 1.000000000000000000, 0.8660254037844387076, 1.000000000000000000, 0.8660254037844387076, 1.000000000000000000, 0.8660254037844387076, 1.000000000000000000, 0.8660254037844387076, 1.000000000000000000, 0.8660254037844387076, 1.000000000000000000, 0.8660254037844387076, 1.000000000000000000, 0.8660254037844387076, 1.000000000000000000, 0.8660254037844387076, 1.000000000000000000, 0.8660254037844387076, 1.000000000000000000, 0.9111405360107203144, 0.9401542295229963209),
 ( 1.000000000000000000, 0.8660254037844387076, 1.000000000000000000, 0.8660254037844387076, 1.000000000000000000, 0.8660254037844387076, 1.000000000000000000, 0.8660254037844387076, 1.000000000000000000, 0.8660254037844387076, 1.000000000000000000, 0.8660254037844387076, 1.000000000000000000, 0.8660254037844387076, 1.000000000000000000, 0.8660254037844387076, 1.000000000000000000, 0.8660254037844387076, 1.000000000000000000, 0.8660254037844387076, 1.000000000000000000, 0.8660254037844387076, 1.000000000000000000, 0.8660254037844387076, 1.000000000000000000, 0.8660254037844387076, 1.000000000000000000, 0.8660254037844387076, 1.000000000000000000, 0.8660254037844387076, 1.000000000000000000, 0.8660254037844387076, 1.000000000000000000, 0.8660254037844387076, 1.000000000000000000, 0.8660254037844387076, 1.000000000000000000, 0.8660254037844387076, 1.000000000000000000, 0.8660254037844387076, 1.000000000000000000, 0.8660254037844387076, 1.000000000000000000, 0.8660254037844387076, 1.000000000000000000, 0.8660254037844387076, 1.000000000000000000, 0.8660254037844387076, 1.000000000000000000, 0.8660254037844387076, 1.000000000000000000, 0.8660254037844387076, 1.000000000000000000, 0.8660254037844387076, 1.000000000000000000, 0.8660254037844387076, 1.000000000000000000, 0.8660254037844387076, 1.000000000000000000, 0.8660254037844387076, 1.000000000000000000, 0.8660254037844387076, 1.000000000000000000, 0.8660254037844387076, 1.000000000000000000, 0.8660254037844387076, 1.000000000000000000, 0.8660254037844387076, 1.000000000000000000, 0.8660254037844387076, 1.000000000000000000, 0.8660254037844387076, 1.000000000000000000, 0.8660254037844387076, 1.000000000000000000, 0.8660254037844387076, 1.000000000000000000, 0.8660254037844387076, 1.000000000000000000, 0.8660254037844387076, 1.000000000000000000, 0.8660254037844387076, 1.000000000000000000, 0.8660254037844387076, 1.000000000000000000, 0.8660254037844387076, 1.000000000000000000, 0.8660254037844387076, 1.000000000000000000, 0.8660254037844387076, 1.000000000000000000, 0.8660254037844387076, 1.000000000000000000, 0.8660254037844387076, 1.000000000000000000, 0.8660254037844387076, 1.000000000000000000, 0.8660254037844387076, 1.000000000000000000, 0.8660254037844387076, 1.000000000000000000, 0.8660254037844387076, 1.000000000000000000, 0.8660254037844387076, 1.000000000000000000, 0.8660254037844387076, 1.000000000000000000, 0.8660254037844387076, 1.000000000000000000, 0.8660254037844387076, 1.000000000000000000, 0.8660254037844387076, 1.000000000000000000, 0.8660254037844387076, 1.000000000000000000, 0.8660254037844387076, 1.000000000000000000, 0.8660254037844387076, 1.000000000000000000, 0.8660254037844387076, 1.000000000000000000, 0.8660254037844387076, 1.000000000000000000, 0.8660254037844387076, 1.000000000000000000, 0.8660254037844387076, 1.000000000000000000, 0.8660254037844387076, 1.000000000000000000, 0.8660254037844387076, 1.000000000000000000, 0.8660254037844387076, 1.000000000000000000, 0.9111405360107203144, 0.9401542295229963209) ) ) 
 REPRESENTATION_ITEM ( '' )  SURFACE ( )  );
#15460 = CARTESIAN_POINT ( 'NONE',  ( -85.40000000000000568, -33.54374999877096286, 99.99999999999998579 ) ) ;
#15461 = CARTESIAN_POINT ( 'NONE',  ( -79.39999999999999147, -34.72106250001229455, 99.99999999999998579 ) ) ;
#15462 = CARTESIAN_POINT ( 'NONE',  ( -82.40000000000000568, -32.08124999877097139, -97.00000000000000000 ) ) ;
#15463 = DIRECTION ( 'NONE',  ( 0.000000000000000000, -1.000000000000000000, 0.000000000000000000 ) ) ;
#15464 = CARTESIAN_POINT ( 'NONE',  ( 79.64356964374998427, -32.69062499938548427, -98.40857419181659793 ) ) ;
#15465 = CARTESIAN_POINT ( 'NONE',  ( 79.39999999999999147, -33.78750000000000853, 101.7320508075688963 ) ) ;
#15466 = CARTESIAN_POINT ( 'NONE',  ( -79.64356964375001269, -34.00312499938549138, 101.5914258081833879 ) ) ;
#15467 = VECTOR ( 'NONE', #18712, 1000.000000000000000 ) ;
#15468 = CARTESIAN_POINT ( 'NONE',  ( 85.15643035625001289, -33.29062499938547859, -99.99999999999998579 ) ) ;
#15469 = ORIENTED_EDGE ( 'NONE', *, *, #15736, .F. ) ;
#15470 = CARTESIAN_POINT ( 'NONE',  ( 235.5999999999999943, -31.61249999999999716, -48.26794919243124582 ) ) ;
#15471 = CARTESIAN_POINT ( 'NONE',  ( -82.39999999999999147, -33.93750000000000000, 103.4641016151377499 ) ) ;
#15472 = DIRECTION ( 'NONE',  ( -1.000000000000000000, -0.000000000000000000, -0.000000000000000000 ) ) ;
#15473 = CARTESIAN_POINT ( 'NONE',  ( 233.9782151781249411, -33.25312499938547717, 102.3871387122750889 ) ) ;
#15474 = CARTESIAN_POINT ( 'NONE',  ( -85.15643035625001289, -30.25312499938548783, 99.99999999999998579 ) ) ;
#15475 = CARTESIAN_POINT ( 'NONE',  ( 235.3564303562499447, -32.27812499938548285, -50.00000000000011369 ) ) ;
#15476 = CARTESIAN_POINT ( 'NONE',  ( -85.40000000000000568, -31.76249999999999929, 101.7320508075688679 ) ) ;
#15477 = ORIENTED_EDGE ( 'NONE', *, *, #8517, .F. ) ;
#15478 = CARTESIAN_POINT ( 'NONE',  ( -79.77811200999879304, -35.00000000000000000, -99.14934632385212865 ) ) ;
#15479 = VECTOR ( 'NONE', #2457, 1000.000000000000000 ) ;
#15480 = CARTESIAN_POINT ( 'NONE',  ( 4.050823680195223098, 2.400527758044901372, 2.978030508226147344 ) ) ;
#15481 = CARTESIAN_POINT ( 'NONE',  ( 79.64356964375001269, -32.65312499938548285, 98.40857419181659793 ) ) ;
#15482 = CARTESIAN_POINT ( 'NONE',  ( 230.1700715539191719, -31.99999999999998579, -51.31340704031387645 ) ) ;
#15483 = CARTESIAN_POINT ( 'NONE',  ( -85.15643035625001289, -30.25312499938548783, 99.99999999999998579 ) ) ;
#15484 = DIRECTION ( 'NONE',  ( 1.000000000000000000, 0.000000000000000000, 0.000000000000000000 ) ) ;
#15485 = CARTESIAN_POINT ( 'NONE',  ( 85.15643035625001289, -34.75312499938548427, 99.99999999999998579 ) ) ;
#15486 =( GEOMETRIC_REPRESENTATION_CONTEXT ( 3 ) GLOBAL_UNCERTAINTY_ASSIGNED_CONTEXT ( ( #9382 ) ) GLOBAL_UNIT_ASSIGNED_CONTEXT ( ( #7132, #16022, #5675 ) ) REPRESENTATION_CONTEXT ( 'NONE', 'WORKASPACE' ) );
#15487 = CARTESIAN_POINT ( 'NONE',  ( 79.64356964375001269, -32.76562499938548711, -101.5914258081833879 ) ) ;
#15488 = EDGE_CURVE ( 'NONE', #4491, #8584, #7383, .T. ) ;
#15489 = CARTESIAN_POINT ( 'NONE',  ( 233.9782151781249411, -30.44062499938548072, -47.61286128772501769 ) ) ;
#15490 = CARTESIAN_POINT ( 'NONE',  ( -85.15643035625001289, -34.79062499938548569, 98.40857419181659793 ) ) ;
#15491 = CARTESIAN_POINT ( 'NONE',  ( -81.02178482187500208, -33.55312499938548854, -102.3871387122750889 ) ) ;
#15492 = VERTEX_POINT ( 'NONE', #17843 ) ;
#15493 = CARTESIAN_POINT ( 'NONE',  ( 85.15643035625001289, -32.95312499938548711, 99.99999999999998579 ) ) ;
#15494 = CARTESIAN_POINT ( 'NONE',  ( 4.052424581287746186, -3.786734753435270662, -0.5771415817959170136 ) ) ;
#15495 = CARTESIAN_POINT ( 'NONE',  ( -83.77821517812500929, -30.51562499938548711, 102.3871387122750889 ) ) ;
#15496 = CARTESIAN_POINT ( 'NONE',  ( -85.15643035624999868, -35.22676555956768141, 98.99674139749697588 ) ) ;
#15497 = CARTESIAN_POINT ( 'NONE',  ( 110.0000000000000000, 10.19999999999997620, -139.9999999999999716 ) ) ;
#15498 = ORIENTED_EDGE ( 'NONE', *, *, #12826, .F. ) ;
#15499 = CARTESIAN_POINT ( 'NONE',  ( -83.90000000000000568, -33.07500000000000284, -97.40192378864668399 ) ) ;
#15500 = PRODUCT_DEFINITION_FORMATION_WITH_SPECIFIED_SOURCE ( 'ANY', '', #12465, .NOT_KNOWN. ) ;
#15501 = CARTESIAN_POINT ( 'NONE',  ( 231.7961524227065695, -34.53615380933862866, -53.00000000000011369 ) ) ;
#15502 = CARTESIAN_POINT ( 'NONE',  ( -83.20384757729335945, -30.09240381056766722, 96.99999999999998579 ) ) ;
#15503 = CARTESIAN_POINT ( 'NONE',  ( -85.15643035625001289, -35.22676544108147567, -101.0032535741825654 ) ) ;
#15504 = CARTESIAN_POINT ( 'NONE',  ( 232.5999999999999375, -34.86562499938548143, 96.81714838363319586 ) ) ;
#15505 = CARTESIAN_POINT ( 'NONE',  ( -85.40000000000000568, -34.41018749875868821, 101.7320508075688679 ) ) ;
#15506 = CARTESIAN_POINT ( 'NONE',  ( -83.77821517812500929, -34.82812499938548711, 97.61286128772489690 ) ) ;
#15507 = CARTESIAN_POINT ( 'NONE',  ( 99.99999999999994316, -32.00000000000000000, -150.0000000000000000 ) ) ;
#15508 = FACE_OUTER_BOUND ( 'NONE', #18968, .T. ) ;
#15509 = CARTESIAN_POINT ( 'NONE',  ( 83.20384757729338787, -34.53615380933862866, -97.00000000000000000 ) ) ;
#15510 =( BOUNDED_CURVE ( )  B_SPLINE_CURVE ( 2, ( #4190, #10150, #4000, #7214, #5576, #17293, #19139, #1267, #5380, #9767, #3798, #3897, #2720, #15825, #5668, #12982, #18761, #887, #14534, #16112, #7126, #2435, #12888, #13078, #15729, #18953, #14344, #1071, #982, #19044, #8680, #11523, #4093, #7028, #10055, #6937, #11425, #18859, #14632, #16015, #8480, #5479, #17386, #14248, #6847, #13168, #2523, #5756, #17194, #12792, #9964, #15918, #6141, #15025, #10626, #291, #17777, #7405, #14825, #10252, #14727, #8867, #5950, #1645, #16214, #1363, #11897, #13551, #17963, #19238, #11706, #191, #4573, #1452, #4384, #2915, #10341, #16305, #17674, #10531, #13368, #1734, #12092 ),
 .UNSPECIFIED., .F., .F. ) 
 B_SPLINE_CURVE_WITH_KNOTS ( ( 3, 2, 2, 2, 2, 2, 2, 2, 2, 2, 2, 2, 2, 2, 2, 2, 2, 2, 2, 2, 2, 2, 2, 2, 2, 2, 2, 2, 2, 2, 2, 2, 2, 2, 2, 2, 2, 2, 2, 2, 2, 3 ),
 ( 0.3716916592826018384, 0.3750191855951751640, 0.3900199530189821795, 0.4050207204427892504, 0.4200214878665962659, 0.4350222552904032813, 0.4500230227142102968, 0.4650237901380173122, 0.4800245575618242722, 0.4950253249856313431, 0.5100260924094384141, 0.5250268598332453740, 0.5400276272570523339, 0.5550283946808594049, 0.5700291621046664758, 0.5850299295284734358, 0.6000306969522805067, 0.6150314643760874667, 0.6300322317998945376, 0.6450329992237016086, 0.6600337666475086795, 0.6750345340713155284, 0.6900353014951225994, 0.7050360689189296703, 0.7200368363427366303, 0.7350376037665437012, 0.7500383711903506612, 0.7650391386141577321, 0.7800399060379648031, 0.7950406734617717630, 0.8100414408855787229, 0.8250422083093857939, 0.8400429757331928649, 0.8550437431569998248, 0.8700445105808067847, 0.8850452780046138557, 0.9000460454284209266, 0.9150468128522278866, 0.9300475802760349575, 0.9450483476998419174, 0.9600491151236488774, 0.9717223562348830113 ),
 .UNSPECIFIED. ) 
 CURVE ( )  GEOMETRIC_REPRESENTATION_ITEM ( )  RATIONAL_B_SPLINE_CURVE ( ( 0.9537471549767081447, 0.9702812541832923632, 1.000000000000000000, 0.8660254037844387076, 1.000000000000000000, 0.8660254037844387076, 1.000000000000000000, 0.8660254037844387076, 1.000000000000000000, 0.8660254037844387076, 1.000000000000000000, 0.8660254037844387076, 1.000000000000000000, 0.8660254037844387076, 1.000000000000000000, 0.8660254037844387076, 1.000000000000000000, 0.8660254037844387076, 1.000000000000000000, 0.8660254037844387076, 1.000000000000000000, 0.8660254037844387076, 1.000000000000000000, 0.8660254037844387076, 1.000000000000000000, 0.8660254037844387076, 1.000000000000000000, 0.8660254037844387076, 1.000000000000000000, 0.8660254037844387076, 1.000000000000000000, 0.8660254037844387076, 1.000000000000000000, 0.8660254037844387076, 1.000000000000000000, 0.8660254037844387076, 1.000000000000000000, 0.8660254037844387076, 1.000000000000000000, 0.8660254037844387076, 1.000000000000000000, 0.8660254037844387076, 1.000000000000000000, 0.8660254037844387076, 1.000000000000000000, 0.8660254037844387076, 1.000000000000000000, 0.8660254037844387076, 1.000000000000000000, 0.8660254037844387076, 1.000000000000000000, 0.8660254037844387076, 1.000000000000000000, 0.8660254037844387076, 1.000000000000000000, 0.8660254037844387076, 1.000000000000000000, 0.8660254037844387076, 1.000000000000000000, 0.8660254037844387076, 1.000000000000000000, 0.8660254037844387076, 1.000000000000000000, 0.8660254037844387076, 1.000000000000000000, 0.8660254037844387076, 1.000000000000000000, 0.8660254037844387076, 1.000000000000000000, 0.8660254037844387076, 1.000000000000000000, 0.8660254037844387076, 1.000000000000000000, 0.8660254037844387076, 1.000000000000000000, 0.8660254037844387076, 1.000000000000000000, 0.8660254037844387076, 1.000000000000000000, 0.8660254037844387076, 1.000000000000000000, 0.8957441496011429027, 0.9537471549767118084 ) ) 
 REPRESENTATION_ITEM ( '' )  );
#15511 = DIRECTION ( 'NONE',  ( -0.000000000000000000, -1.000000000000000000, -0.000000000000000000 ) ) ;
#15512 = CIRCLE ( 'NONE', #10514, 2.649999999999982148 ) ;
#15513 = CARTESIAN_POINT ( 'NONE',  ( 79.64356964375001269, -31.86562499938548143, -101.5914258081833879 ) ) ;
#15514 = CARTESIAN_POINT ( 'NONE',  ( 230.9855258467272563, -35.02670941564509377, 97.25687757881057394 ) ) ;
#15515 = ORIENTED_EDGE ( 'NONE', *, *, #6312, .F. ) ;
#15516 = CARTESIAN_POINT ( 'NONE',  ( 232.5999999999999943, -34.64062499938548001, -46.81714838363331666 ) ) ;
#15517 = APPLICATION_PROTOCOL_DEFINITION ( 'draft international standard', 'automotive_design', 1998, #7067 ) ;
#15518 = CARTESIAN_POINT ( 'NONE',  ( 232.5999999999999375, -33.51562499938548001, 96.81714838363319586 ) ) ;
#15519 = CARTESIAN_POINT ( 'NONE',  ( 229.5999999999999375, -34.93124999877095860, -51.73205080756898866 ) ) ;
#15520 = AXIS2_PLACEMENT_3D ( 'NONE', #4368, #13444, #11789 ) ;
#15521 = CARTESIAN_POINT ( 'NONE',  ( -85.15643035624999868, -32.87812499938549138, 98.40857419181659793 ) ) ;
#15522 = CARTESIAN_POINT ( 'NONE',  ( 232.5999999999999375, -34.83749999999999147, -47.00000000000011369 ) ) ;
#15523 = ORIENTED_EDGE ( 'NONE', *, *, #111, .T. ) ;
#15524 = ORIENTED_EDGE ( 'NONE', *, *, #9846, .T. ) ;
#15525 = CARTESIAN_POINT ( 'NONE',  ( -85.15643035624999868, -31.52812499938547930, -101.5914258081833879 ) ) ;
#15526 = CYLINDRICAL_SURFACE ( 'NONE', #2868, 3.000000000000002665 ) ;
#15527 = ORIENTED_EDGE ( 'NONE', *, *, #16544, .F. ) ;
#15528 = CARTESIAN_POINT ( 'NONE',  ( 81.02178482187500208, -34.60312499938549280, 97.61286128772489690 ) ) ;
#15529 = VECTOR ( 'NONE', #14766, 1000.000000000000000 ) ;
#15530 = CARTESIAN_POINT ( 'NONE',  ( -82.39999999999999147, -33.65624999877096712, -103.4641016151377499 ) ) ;
#15531 = CARTESIAN_POINT ( 'NONE',  ( 80.90000000000000568, -32.85000000000000142, 102.5980762113533018 ) ) ;
#15532 = CARTESIAN_POINT ( 'NONE',  ( -79.39999999999999147, -33.82500000000000284, 99.99999999999998579 ) ) ;
#15533 = CARTESIAN_POINT ( 'NONE',  ( -79.39999999999999147, -31.06874999877096855, 99.99999999999998579 ) ) ;
#15534 = CARTESIAN_POINT ( 'NONE',  ( -82.39999999999999147, -33.65624999877096712, 96.53589838486223584 ) ) ;
#15535 = CIRCLE ( 'NONE', #14580, 0.4999999999999978351 ) ;
#15536 = CARTESIAN_POINT ( 'NONE',  ( 84.59935209580758908, -34.99999999999999289, -101.7928000422457728 ) ) ;
#15537 = MECHANICAL_DESIGN_GEOMETRIC_PRESENTATION_REPRESENTATION (  '', ( #7111 ), #1191 ) ;
#15538 = PLANE ( 'NONE',  #18325 ) ;
#15539 = CARTESIAN_POINT ( 'NONE',  ( 234.5796347213265278, -32.00000000000000711, 102.1983759483905772 ) ) ;
#15540 = CARTESIAN_POINT ( 'NONE',  ( 232.5999999999999375, -34.52812499938548285, 103.1828516163667899 ) ) ;
#15541 = ORIENTED_EDGE ( 'NONE', *, *, #3943, .T. ) ;
#15542 = CARTESIAN_POINT ( 'NONE',  ( 84.05108659120821812, -32.00820041275123629, -97.77040367152264366 ) ) ;
#15543 = FILL_AREA_STYLE ('',( #9870 ) ) ;
#15544 = CARTESIAN_POINT ( 'NONE',  ( -84.51154815724953551, -35.14114861271051637, -101.7717992799616553 ) ) ;
#15545 = CARTESIAN_POINT ( 'NONE',  ( 4.175572532730932096, 4.122058607836115662, 6.089476485528261042E-15 ) ) ;
#15546 = ORIENTED_EDGE ( 'NONE', *, *, #14987, .F. ) ;
#15547 = FACE_OUTER_BOUND ( 'NONE', #10859, .T. ) ;
#15548 = CARTESIAN_POINT ( 'NONE',  ( 0.000000000000000000, 0.000000000000000000, 0.000000000000000000 ) ) ;
#15549 = PLANE ( 'NONE',  #2869 ) ;
#15550 = VERTEX_POINT ( 'NONE', #4456 ) ;
#15551 = CARTESIAN_POINT ( 'NONE',  ( 111.5000000000000142, 12.69999999999998508, 50.00000000000001421 ) ) ;
#15552 = AXIS2_PLACEMENT_3D ( 'NONE', #6528, #10030, #7001 ) ;
#15553 = CARTESIAN_POINT ( 'NONE',  ( 4.114405500665267112, -2.025575754679707075, 3.508400121684927431 ) ) ;
#15554 = EDGE_LOOP ( 'NONE', ( #17876, #16697, #10566, #4646, #3140, #16798, #12149 ) ) ;
#15555 = CARTESIAN_POINT ( 'NONE',  ( 80.90000000000000568, -33.24374999877097281, -97.40192378864668399 ) ) ;
#15556 = CARTESIAN_POINT ( 'NONE',  ( 83.77821517812500929, -34.71562499938548285, -97.61286128772489690 ) ) ;
#15557 = CYLINDRICAL_SURFACE ( 'NONE', #11103, 3.000000000000002665 ) ;
#15558 = CARTESIAN_POINT ( 'NONE',  ( -82.39999999999999147, -30.36562499938549209, 96.81714838363319586 ) ) ;
#15559 = CARTESIAN_POINT ( 'NONE',  ( -85.40000000000000568, -30.03750000000000497, 98.26794919243111792 ) ) ;
#15560 = DIRECTION ( 'NONE',  ( 0.000000000000000000, -1.000000000000000000, 0.000000000000000000 ) ) ;
#15561 = DIRECTION ( 'NONE',  ( -0.000000000000000000, 1.000000000000000000, -0.000000000000000000 ) ) ;
#15562 = CARTESIAN_POINT ( 'NONE',  ( 85.15643035625001289, -32.54062499938548569, -98.40857419181659793 ) ) ;
#15563 = AXIS2_PLACEMENT_3D ( 'NONE', #11499, #10034, #1430 ) ;
#15564 = CARTESIAN_POINT ( 'NONE',  ( -80.90000000000000568, -33.84374999877096712, 102.5980762113533018 ) ) ;
#15565 = CARTESIAN_POINT ( 'NONE',  ( -83.77821517812500929, -34.26562499938548711, 97.61286128772489690 ) ) ;
#15566 = EDGE_CURVE ( 'NONE', #12940, #17012, #10411, .T. ) ;
#15567 = DIRECTION ( 'NONE',  ( 0.000000000000000000, 0.000000000000000000, 1.000000000000000000 ) ) ;
#15568 = ORIENTED_EDGE ( 'NONE', *, *, #7133, .F. ) ;
#15569 = CARTESIAN_POINT ( 'NONE',  ( 234.0999999999999375, -32.04374999877096286, -47.40192378864679768 ) ) ;
#15570 = CARTESIAN_POINT ( 'NONE',  ( -85.40000000000000568, -33.63750000000000284, 98.26794919243111792 ) ) ;
#15571 = CARTESIAN_POINT ( 'NONE',  ( 4.000000000000000000, 2.309401076758497151, -5.000000000000000000 ) ) ;
#15572 = CARTESIAN_POINT ( 'NONE',  ( 231.2217848218749339, -33.02812499938547575, 97.61286128772489690 ) ) ;
#15573 = CARTESIAN_POINT ( 'NONE',  ( -79.64356964375001269, -30.89062499938548711, 98.40857419181659793 ) ) ;
#15574 = CARTESIAN_POINT ( 'NONE',  ( 233.9782151781249411, -31.19062499938547717, -52.38713871227520968 ) ) ;
#15575 = CARTESIAN_POINT ( 'NONE',  ( -80.90000000000000568, -32.40000000000000568, 97.40192378864668399 ) ) ;
#15576 = ADVANCED_FACE ( 'NONE', ( #16191, #6024 ), #15098, .F. ) ;
#15577 = VERTEX_POINT ( 'NONE', #12070 ) ;
#15578 =( REPRESENTATION_RELATIONSHIP ('NONE','NONE', #14468, #4499 ) REPRESENTATION_RELATIONSHIP_WITH_TRANSFORMATION ( #11311 )SHAPE_REPRESENTATION_RELATIONSHIP( ) );
#15579 = CARTESIAN_POINT ( 'NONE',  ( 4.086262418390198548, -2.102635014057360863, 3.500000000000000444 ) ) ;
#15580 = CARTESIAN_POINT ( 'NONE',  ( 82.85452780460276756, -34.99999999999997868, 97.27546421900271412 ) ) ;
#15581 = CARTESIAN_POINT ( 'NONE',  ( 79.64356964375001269, -31.30312499938548854, 98.40857419181659793 ) ) ;
#15582 = CARTESIAN_POINT ( 'NONE',  ( 230.1427008797911924, -31.99999999999998579, -48.73859666561349968 ) ) ;
#15583 = EDGE_CURVE ( 'NONE', #11146, #5933, #9133, .T. ) ;
#15584 = CARTESIAN_POINT ( 'NONE',  ( -85.15643035625001289, -34.30312499938548854, 99.99999999999998579 ) ) ;
#15585 = CARTESIAN_POINT ( 'NONE',  ( -82.39999999999999147, -32.81250000000000000, 97.00000000000000000 ) ) ;
#15586 = CARTESIAN_POINT ( 'NONE',  ( 83.77821517812500929, -32.31562499938548427, 97.61286128772489690 ) ) ;
#15587 = ADVANCED_FACE ( 'NONE', ( #7577 ), #124, .F. ) ;
#15588 = CARTESIAN_POINT ( 'NONE',  ( 83.77821517812500929, -32.12812499938548427, -97.61286128772489690 ) ) ;
#15589 = CARTESIAN_POINT ( 'NONE',  ( 235.3564303562499447, -33.51562499938548001, -50.00000000000011369 ) ) ;
#15590 = CARTESIAN_POINT ( 'NONE',  ( -79.64356964374998427, -34.04062499938549280, 98.40857419181659793 ) ) ;
#15591 = CARTESIAN_POINT ( 'NONE',  ( -79.64356964375001269, -31.30312499938548854, -98.40857419181659793 ) ) ;
#15592 = ADVANCED_FACE ( 'NONE', ( #11454 ), #6778, .F. ) ;
#15593 = ORIENTED_EDGE ( 'NONE', *, *, #3547, .F. ) ;
#15594 = CARTESIAN_POINT ( 'NONE',  ( 82.39999999999999147, -33.06562499938548427, 103.1828516163667899 ) ) ;
#15595 = CARTESIAN_POINT ( 'NONE',  ( 4.086376042167609413, -4.082715877136871008, 0.07147133206917888337 ) ) ;
#15596 = CARTESIAN_POINT ( 'NONE',  ( -85.15643035624999868, -31.97812499938548925, 98.40857419181659793 ) ) ;
#15597 = CARTESIAN_POINT ( 'NONE',  ( -79.64356964374999848, -34.97812499938548569, 99.99999999999998579 ) ) ;
#15598 = CARTESIAN_POINT ( 'NONE',  ( 83.20384757729335945, -34.85759618943233562, 96.99999999999998579 ) ) ;
#15599 = ORIENTED_EDGE ( 'NONE', *, *, #7932, .F. ) ;
#15600 = CARTESIAN_POINT ( 'NONE',  ( -79.39999999999999147, -33.33749999999999858, -101.7320508075688821 ) ) ;
#15601 = PRODUCT_DEFINITION_SHAPE ( 'NONE', 'NONE',  #19327 ) ;
#15602 = FACE_OUTER_BOUND ( 'NONE', #17744, .T. ) ;
#15603 = CARTESIAN_POINT ( 'NONE',  ( 231.5800379434388674, -35.00000000000000000, -52.82826157480266005 ) ) ;
#15604 = EDGE_CURVE ( 'NONE', #15250, #10850, #5213, .T. ) ;
#15605 = CARTESIAN_POINT ( 'NONE',  ( -80.90000000000000568, -32.94374999877096855, 102.5980762113533018 ) ) ;
#15606 = CARTESIAN_POINT ( 'NONE',  ( 231.2217848218749339, -30.66562499938547859, 97.61286128772489690 ) ) ;
#15607 = CARTESIAN_POINT ( 'NONE',  ( -82.39999999999999147, -34.78518749875867400, 103.4641016151377499 ) ) ;
#15608 = DIRECTION ( 'NONE',  ( 0.000000000000000000, -1.000000000000000000, 0.000000000000000000 ) ) ;
#15609 = CARTESIAN_POINT ( 'NONE',  ( -69.99999999999998579, -32.00000000000000000, 150.0000000000000000 ) ) ;
#15610 = CARTESIAN_POINT ( 'NONE',  ( 249.9999999999999716, -29.80000000000000426, -100.0000000000000000 ) ) ;
#15611 = CARTESIAN_POINT ( 'NONE',  ( 83.77821517812500929, -30.32812499938548711, 102.3871387122750889 ) ) ;
#15612 = CARTESIAN_POINT ( 'NONE',  ( 232.5999999999999375, -29.99999999999999645, 99.99999999999998579 ) ) ;
#15613 = CARTESIAN_POINT ( 'NONE',  ( 83.77821517812500929, -31.52812499938548996, -102.3871387122750889 ) ) ;
#15614 = CARTESIAN_POINT ( 'NONE',  ( 0.000000000000000000, 0.000000000000000000, 0.000000000000000000 ) ) ;
#15615 = ORIENTED_EDGE ( 'NONE', *, *, #14583, .T. ) ;
#15616 = CARTESIAN_POINT ( 'NONE',  ( 79.39999999999999147, -31.55624999877096926, 98.26794919243113213 ) ) ;
#15617 = CARTESIAN_POINT ( 'NONE',  ( 229.8435696437499303, -31.60312499938548214, 99.99999999999998579 ) ) ;
#15618 = EDGE_CURVE ( 'NONE', #7254, #3907, #15661, .T. ) ;
#15619 = CARTESIAN_POINT ( 'NONE',  ( 233.9782151781249411, -34.15312499938547575, -47.61286128772501769 ) ) ;
#15620 = CARTESIAN_POINT ( 'NONE',  ( -79.64356964375001269, -33.92812499938548854, 98.40857419181659793 ) ) ;
#15621 = CARTESIAN_POINT ( 'NONE',  ( 85.40000000000000568, -34.01250000000000284, 98.26794919243111792 ) ) ;
#15622 = ORIENTED_EDGE ( 'NONE', *, *, #4723, .F. ) ;
#15623 = ORIENTED_EDGE ( 'NONE', *, *, #8740, .T. ) ;
#15624 = CARTESIAN_POINT ( 'NONE',  ( -83.77821517812500929, -30.51562499938548711, -97.61286128772489690 ) ) ;
#15625 = PLANE ( 'NONE',  #7552 ) ;
#15626 = ORIENTED_EDGE ( 'NONE', *, *, #15093, .F. ) ;
#15627 = CARTESIAN_POINT ( 'NONE',  ( 79.64356964374998427, -33.59062499938548285, 101.5914258081833879 ) ) ;
#15628 = CARTESIAN_POINT ( 'NONE',  ( -85.40000000000000568, -33.09374999877096712, -99.99999999999998579 ) ) ;
#15629 =( BOUNDED_CURVE ( )  B_SPLINE_CURVE ( 2, ( #7901, #11118, #11023, #2037, #6447, #10736, #3502, #17086, #7997 ),
 .UNSPECIFIED., .F., .F. ) 
 B_SPLINE_CURVE_WITH_KNOTS ( ( 3, 2, 2, 2, 3 ),
 ( 0.06250000000000006939, 0.06944444444444444753, 0.08333333333333332871, 0.09722222222222222376, 0.1041666666666666713 ),
 .UNSPECIFIED. ) 
 CURVE ( )  GEOMETRIC_REPRESENTATION_ITEM ( )  RATIONAL_B_SPLINE_CURVE ( ( 0.9330127018922194093, 0.9330127018922200755, 1.000000000000000000, 0.8660254037844387076, 1.000000000000000000, 0.8660254037844387076, 1.000000000000000000, 0.9330127018922192983, 0.9330127018922194093 ) ) 
 REPRESENTATION_ITEM ( '' )  );
#15630 = CARTESIAN_POINT ( 'NONE',  ( 80.90000000000000568, -33.45000000000000284, 97.40192378864668399 ) ) ;
#15631 = CARTESIAN_POINT ( 'NONE',  ( -80.90000000000000568, -32.10000000000000142, 102.5980762113533018 ) ) ;
#15632 = CARTESIAN_POINT ( 'NONE',  ( -85.40000000000000568, -33.09374999877096712, 99.99999999999998579 ) ) ;
#15633 = CARTESIAN_POINT ( 'NONE',  ( -79.39999999999999147, -34.25624999877096855, 101.7320508075688537 ) ) ;
#15634 = DIRECTION ( 'NONE',  ( 1.000000000000000000, -1.387778780781445676E-15, -2.407412430484046130E-31 ) ) ;
#15635 = CARTESIAN_POINT ( 'NONE',  ( 244.7999999999999545, -29.80000000000002203, 147.7999999999999829 ) ) ;
#15636 = CARTESIAN_POINT ( 'NONE',  ( -82.40000000000000568, -34.10624999877096997, 96.99999999999998579 ) ) ;
#15637 = CARTESIAN_POINT ( 'NONE',  ( 235.3564303562499447, -34.82812499938548001, 98.40857419181659793 ) ) ;
#15638 = EDGE_LOOP ( 'NONE', ( #14266, #1064 ) ) ;
#15639 = CARTESIAN_POINT ( 'NONE',  ( 82.39999999999999147, -33.17812499938548854, -103.1828516163667899 ) ) ;
#15640 =( NAMED_UNIT ( * ) SI_UNIT ( $, .STERADIAN. ) SOLID_ANGLE_UNIT ( ) );
#15641 = CARTESIAN_POINT ( 'NONE',  ( -79.64356964374999848, -34.86562499938548143, -99.99999999999998579 ) ) ;
#15642 = CARTESIAN_POINT ( 'NONE',  ( 235.5999999999999375, -30.61874999877096215, -50.00000000000011369 ) ) ;
#15643 = ORIENTED_EDGE ( 'NONE', *, *, #12453, .T. ) ;
#15644 = CARTESIAN_POINT ( 'NONE',  ( 244.7999999999999545, -29.80000000000000426, 150.0000000000000000 ) ) ;
#15645 = CARTESIAN_POINT ( 'NONE',  ( -6.259644161404860030E-16, -4.618802153517027165, -3.433295621305388234 ) ) ;
#15646 = PLANE ( 'NONE',  #9415 ) ;
#15647 = VERTEX_POINT ( 'NONE', #5606 ) ;
#15648 = CARTESIAN_POINT ( 'NONE',  ( 3.948103430090709409, -2.682758828852222166, 2.353325403973829388 ) ) ;
#15649 = CARTESIAN_POINT ( 'NONE',  ( 4.175813232069147674, -2.061359961916367833, 3.570380186727398542 ) ) ;
#15650 = ORIENTED_EDGE ( 'NONE', *, *, #12448, .T. ) ;
#15651 = DIRECTION ( 'NONE',  ( 1.000000000000000000, 0.000000000000000000, 0.000000000000000000 ) ) ;
#15652 = CARTESIAN_POINT ( 'NONE',  ( 83.90000000000000568, -33.67500000000000426, -97.40192378864668399 ) ) ;
#15653 = CYLINDRICAL_SURFACE ( 'NONE', #16107, 3.000000000000002665 ) ;
#15654 = CARTESIAN_POINT ( 'NONE',  ( -83.90000000000000568, -34.06874999877096855, 97.40192378864668399 ) ) ;
#15655 = CARTESIAN_POINT ( 'NONE',  ( -83.90000000000000568, -30.52500000000000213, 97.40192378864668399 ) ) ;
#15656 = DIRECTION ( 'NONE',  ( 1.000000000000000000, -9.941108744852765039E-17, 1.788378118793199314E-31 ) ) ;
#15657 = FACE_OUTER_BOUND ( 'NONE', #16268, .T. ) ;
#15658 = CARTESIAN_POINT ( 'NONE',  ( 81.02178482187500208, -34.60312499938549280, -102.3871387122750889 ) ) ;
#15659 = LINE ( 'NONE', #2266, #1814 ) ;
#15660 = CARTESIAN_POINT ( 'NONE',  ( -79.64356964375001269, -33.10312499938549280, 101.5914258081833879 ) ) ;
#15661 = LINE ( 'NONE', #11160, #17410 ) ;
#15662 = ORIENTED_EDGE ( 'NONE', *, *, #5299, .T. ) ;
#15663 = LINE ( 'NONE', #2273, #11775 ) ;
#15664 = CARTESIAN_POINT ( 'NONE',  ( -79.39999999999999147, -33.41250000000000142, 101.7320508075688537 ) ) ;
#15665 = CLOSED_SHELL ( 'NONE', ( #2295, #5230, #15976, #10438, #10230, #9259, #1821, #16046, #17956, #349, #14984, #5392, #2488, #1947, #3962, #4344, #19162, #14408, #14888, #12470, #10109, #434, #2925, #8744, #16563, #5653, #6246, #18609, #10986 ) ) ;
#15666 = DIRECTION ( 'NONE',  ( 0.000000000000000000, 0.000000000000000000, -1.000000000000000000 ) ) ;
#15667 = CARTESIAN_POINT ( 'NONE',  ( 85.40000000000000568, -33.63750000000000284, 101.7320508075688821 ) ) ;
#15668 = CARTESIAN_POINT ( 'NONE',  ( -82.39999999999999147, -34.86562499938548854, 96.81714838363319586 ) ) ;
#15669 = CARTESIAN_POINT ( 'NONE',  ( 235.3564303562499447, -34.94062499938547717, -51.59142580818350865 ) ) ;
#15670 = B_SPLINE_CURVE_WITH_KNOTS ( 'NONE', 3,
 ( #11849, #4825, #3339, #16348, #1504, #4523 ),
 .UNSPECIFIED., .F., .F.,
 ( 4, 2, 4 ),
 ( -3.640115492410698714E-06, 0.0002066546034003381217, 0.0004169493222930869755 ),
 .UNSPECIFIED. ) ;
#15671 = ORIENTED_EDGE ( 'NONE', *, *, #7478, .F. ) ;
#15672 = CARTESIAN_POINT ( 'NONE',  ( -81.96801452314034009, -35.00000000000001421, -97.27181766474433289 ) ) ;
#15673 = CARTESIAN_POINT ( 'NONE',  ( -82.40000000000000568, -34.55624999877097281, 97.00000000000000000 ) ) ;
#15674 = CARTESIAN_POINT ( 'NONE',  ( 82.39999999999999147, -33.40312499938548285, 103.1828516163667899 ) ) ;
#15675 = CARTESIAN_POINT ( 'NONE',  ( -4.235886605889389145, -2.417314728048544303, -3.751161874094020909 ) ) ;
#15676 = EDGE_CURVE ( 'NONE', #9425, #12925, #6875, .T. ) ;
#15677 = VECTOR ( 'NONE', #4187, 1000.000000000000000 ) ;
#15678 = AXIS2_PLACEMENT_3D ( 'NONE', #16264, #4346, #16650 ) ;
#15679 = DIRECTION ( 'NONE',  ( 0.000000000000000000, -1.000000000000000000, 0.000000000000000000 ) ) ;
#15680 = CARTESIAN_POINT ( 'NONE',  ( -83.77821517812500929, -34.67812499938548854, 102.3871387122750889 ) ) ;
#15681 = CARTESIAN_POINT ( 'NONE',  ( -83.77821517812500929, -32.12812499938548427, -102.3871387122750889 ) ) ;
#15682 = CARTESIAN_POINT ( 'NONE',  ( 85.15643035625001289, -31.04062499938548569, 99.99999999999998579 ) ) ;
#15683 = EDGE_CURVE ( 'NONE', #14034, #18769, #728, .T. ) ;
#15684 = ADVANCED_FACE ( 'NONE', ( #8236 ), #1010, .T. ) ;
#15685 = CARTESIAN_POINT ( 'NONE',  ( 82.39999999999999147, -34.19062499938548427, -103.1828516163667899 ) ) ;
#15686 = CARTESIAN_POINT ( 'NONE',  ( 232.5999999999999375, -32.72812499938547859, -46.81714838363331666 ) ) ;
#15687 = CARTESIAN_POINT ( 'NONE',  ( -85.15643035625001289, -33.40312499938548285, 99.99999999999998579 ) ) ;
#15688 = ORIENTED_EDGE ( 'NONE', *, *, #16573, .F. ) ;
#15689 = CARTESIAN_POINT ( 'NONE',  ( 85.15643035624999868, -32.99062499938548854, 101.5914258081833879 ) ) ;
#15690 = CARTESIAN_POINT ( 'NONE',  ( 235.5999999999999943, -32.83124999877096428, 98.26794919243110371 ) ) ;
#15691 = CARTESIAN_POINT ( 'NONE',  ( -83.90000000000000568, -33.07500000000000284, 102.5980762113533018 ) ) ;
#15692 = VECTOR ( 'NONE', #1163, 1000.000000000000000 ) ;
#15693 = CARTESIAN_POINT ( 'NONE',  ( -82.39999999999999147, -34.19062499938548427, 103.1828516163667899 ) ) ;
#15694 = DIRECTION ( 'NONE',  ( 1.000000000000000000, 0.000000000000000000, -0.000000000000000000 ) ) ;
#15695 = EDGE_LOOP ( 'NONE', ( #3937, #4912, #13687, #374, #5032, #3500 ) ) ;
#15696 = CARTESIAN_POINT ( 'NONE',  ( -83.90000000000000568, -34.12500000000000000, -102.5980762113533018 ) ) ;
#15697 = ADVANCED_FACE ( 'NONE', ( #11355, #17129, #5508 ), #6681, .T. ) ;
#15698 = CARTESIAN_POINT ( 'NONE',  ( 231.0999999999999375, -34.51874999877096428, -52.59807621135342970 ) ) ;
#15699 = CARTESIAN_POINT ( 'NONE',  ( 231.7961524227065695, -34.14240381056765017, -53.00000000000011369 ) ) ;
#15700 = CARTESIAN_POINT ( 'NONE',  ( -85.40000000000000568, -30.03356250001229810, 98.26794919243111792 ) ) ;
#15701 = EDGE_CURVE ( 'NONE', #17884, #422, #4032, .T. ) ;
#15702 = ADVANCED_FACE ( 'NONE', ( #15948 ), #18886, .T. ) ;
#15703 = CARTESIAN_POINT ( 'NONE',  ( -82.39999999999999147, -33.66018749875868110, 96.53589838486223584 ) ) ;
#15704 = CARTESIAN_POINT ( 'NONE',  ( 82.40000000000000568, -34.10624999877096997, -96.99999999999998579 ) ) ;
#15705 = CARTESIAN_POINT ( 'NONE',  ( -82.39999999999999147, -33.43124999877097281, -96.99999999999998579 ) ) ;
#15706 = FACE_OUTER_BOUND ( 'NONE', #15400, .T. ) ;
#15707 = AXIS2_PLACEMENT_3D ( 'NONE', #428, #1872, #18198 ) ;
#15708 = LINE ( 'NONE', #10033, #17391 ) ;
#15709 = CARTESIAN_POINT ( 'NONE',  ( 231.6794753800827777, -34.98323688327302960, -52.93263647803299676 ) ) ;
#15710 = CARTESIAN_POINT ( 'NONE',  ( 85.15643035625001289, -32.05312499938548854, -99.99999999999998579 ) ) ;
#15711 = CARTESIAN_POINT ( 'NONE',  ( 4.132952817037859994, 2.031684012687258623, 3.518979934899746809 ) ) ;
#15712 = EDGE_LOOP ( 'NONE', ( #8634, #8851, #16541, #18126 ) ) ;
#15713 = CARTESIAN_POINT ( 'NONE',  ( 110.0000000000000000, 10.19999999999997620, -145.0000000000000000 ) ) ;
#15714 = CARTESIAN_POINT ( 'NONE',  ( 233.9782151781249411, -33.25312499938547717, 102.3871387122750889 ) ) ;
#15715 = CARTESIAN_POINT ( 'NONE',  ( 232.5999999999999375, -33.96562499938547575, -53.18285161636690361 ) ) ;
#15716 = CARTESIAN_POINT ( 'NONE',  ( -83.77821517812500929, -33.36562499938548854, 97.61286128772489690 ) ) ;
#15717 = CARTESIAN_POINT ( 'NONE',  ( 231.0999999999999375, -32.62499999999999289, -47.40192378864679768 ) ) ;
#15718 = VERTEX_POINT ( 'NONE', #18597 ) ;
#15719 = CARTESIAN_POINT ( 'NONE',  ( -81.02178482187500208, -32.54062499938548569, -102.3871387122750889 ) ) ;
#15720 = PLANE ( 'NONE',  #13479 ) ;
#15721 = ORIENTED_EDGE ( 'NONE', *, *, #6998, .T. ) ;
#15722 = CARTESIAN_POINT ( 'NONE',  ( 85.15643035625001289, -33.44062499938548427, 101.5914258081833879 ) ) ;
#15723 = CARTESIAN_POINT ( 'NONE',  ( -82.39999999999999147, -33.20624999877097139, -103.4641016151377499 ) ) ;
#15724 = CARTESIAN_POINT ( 'NONE',  ( 80.90000000000000568, -34.35000000000000853, 97.40192378864668399 ) ) ;
#15725 = CARTESIAN_POINT ( 'NONE',  ( -99.99999999999998579, 0.000000000000000000, 150.0000000000000000 ) ) ;
#15726 = CARTESIAN_POINT ( 'NONE',  ( -79.39999999999999147, -32.86874999877097281, 99.99999999999998579 ) ) ;
#15727 = ADVANCED_FACE ( 'NONE', ( #5316 ), #14463, .F. ) ;
#15728 = CARTESIAN_POINT ( 'NONE',  ( -82.39999999999999147, -32.39062499938548001, 103.1828516163667899 ) ) ;
#15729 = CARTESIAN_POINT ( 'NONE',  ( -85.15643035625001289, -32.84062499938548285, -99.99999999999998579 ) ) ;
#15730 = CARTESIAN_POINT ( 'NONE',  ( 69.99999999999998579, -31.99999999999998579, 150.0000000000000000 ) ) ;
#15731 = CARTESIAN_POINT ( 'NONE',  ( 232.8441546701661480, -32.00000000000000000, 102.8696726379688755 ) ) ;
#15732 = CARTESIAN_POINT ( 'NONE',  ( 229.5999999999999375, -30.44999999999999574, 99.99999999999998579 ) ) ;
#15733 = ORIENTED_EDGE ( 'NONE', *, *, #13895, .T. ) ;
#15734 = CARTESIAN_POINT ( 'NONE',  ( 0.000000000000000000, 3.031088913245532979, -1.750000000000004219 ) ) ;
#15735 =( LENGTH_UNIT ( ) NAMED_UNIT ( * ) SI_UNIT ( .MILLI., .METRE. ) );
#15736 = EDGE_CURVE ( 'NONE', #14453, #15126, #12597, .T. ) ;
#15737 = CARTESIAN_POINT ( 'NONE',  ( 232.5999999999999375, -30.73124999877096286, 103.4641016151377499 ) ) ;
#15738 = LINE ( 'NONE', #1078, #2428 ) ;
#15739 = ORIENTED_EDGE ( 'NONE', *, *, #11672, .T. ) ;
#15740 = CARTESIAN_POINT ( 'NONE',  ( 83.90000000000000568, -32.62500000000000000, 97.40192378864668399 ) ) ;
#15741 = CARTESIAN_POINT ( 'NONE',  ( -85.15643035625001289, -30.55312499938548143, 101.5914258081833879 ) ) ;
#15742 = DIRECTION ( 'NONE',  ( -0.000000000000000000, -1.000000000000000000, -0.000000000000000000 ) ) ;
#15743 = VERTEX_POINT ( 'NONE', #5413 ) ;
#15744 = CARTESIAN_POINT ( 'NONE',  ( 231.0999999999999375, -33.61874999877096570, 97.40192378864668399 ) ) ;
#15745 = DIRECTION ( 'NONE',  ( -0.000000000000000000, 1.000000000000000000, -0.000000000000000000 ) ) ;
#15746 = EDGE_LOOP ( 'NONE', ( #15814, #16969, #17583, #7040 ) ) ;
#15747 = DIRECTION ( 'NONE',  ( 1.000000000000000000, 0.000000000000000000, 0.000000000000000000 ) ) ;
#15748 = CARTESIAN_POINT ( 'NONE',  ( 80.90000000000000568, -32.10000000000000142, -102.5980762113533018 ) ) ;
#15749 = CARTESIAN_POINT ( 'NONE',  ( 105.2000000000000739, -32.00000000000002842, 147.7999999999999829 ) ) ;
#15750 = CARTESIAN_POINT ( 'NONE',  ( -79.64356964375001269, -30.44062499938548783, 98.40857419181659793 ) ) ;
#15751 = CARTESIAN_POINT ( 'NONE',  ( -83.90000000000000568, -30.07499999999999929, 97.40192378864668399 ) ) ;
#15752 = CARTESIAN_POINT ( 'NONE',  ( -85.40000000000000568, -32.19374999877096855, -99.99999999999998579 ) ) ;
#15753 = CARTESIAN_POINT ( 'NONE',  ( -7.538593230563273018E-17, 0.3423821193476820346, -3.499999999999999556 ) ) ;
#15754 = CARTESIAN_POINT ( 'NONE',  ( 82.39999999999999147, -34.41562499938548569, -96.81714838363319586 ) ) ;
#15755 = DIRECTION ( 'NONE',  ( 0.000000000000000000, 0.000000000000000000, -1.000000000000000000 ) ) ;
#15756 = CARTESIAN_POINT ( 'NONE',  ( -81.02178482187500208, -32.69062499938548427, 102.3871387122750889 ) ) ;
#15757 = DIRECTION ( 'NONE',  ( 1.000000000000000000, 0.000000000000000000, 0.000000000000000000 ) ) ;
#15758 = VERTEX_POINT ( 'NONE', #15858 ) ;
#15759 = CARTESIAN_POINT ( 'NONE',  ( 235.5999999999999943, -33.86249999999999716, -48.26794919243124582 ) ) ;
#15760 = CARTESIAN_POINT ( 'NONE',  ( 234.5119179762161536, -35.00000000000002132, 97.80480077079613466 ) ) ;
#15761 = PRODUCT_DEFINITION_SHAPE ( 'NONE', 'NONE',  #19332 ) ;
#15762 = CARTESIAN_POINT ( 'NONE',  ( 83.20384757729337366, -34.80134618820331127, 97.00000000000000000 ) ) ;
#15763 = CARTESIAN_POINT ( 'NONE',  ( 229.8435696437499587, -34.71562499938547575, 101.5914258081833879 ) ) ;
#15764 = CARTESIAN_POINT ( 'NONE',  ( -82.39999999999999147, -34.41562499938547859, 96.81714838363319586 ) ) ;
#15765 = CARTESIAN_POINT ( 'NONE',  ( 235.3564303562499447, -31.26562499938547646, -50.00000000000011369 ) ) ;
#15766 = VERTEX_POINT ( 'NONE', #8420 ) ;
#15767 = CARTESIAN_POINT ( 'NONE',  ( -81.44590651011453986, -35.00138974199450814, 97.15054881843455803 ) ) ;
#15768 = CARTESIAN_POINT ( 'NONE',  ( -85.15643035624999868, -32.80312499938548854, 101.5914258081833879 ) ) ;
#15769 = CARTESIAN_POINT ( 'NONE',  ( -81.59615242270662350, -34.57634618820329564, 96.99999999999997158 ) ) ;
#15770 = CARTESIAN_POINT ( 'NONE',  ( 85.15643035625001289, -32.84062499938548285, 99.99999999999998579 ) ) ;
#15771 = CARTESIAN_POINT ( 'NONE',  ( -1.287237434361707233, -3.875615274277397937, -3.430618716626816500 ) ) ;
#15772 = AXIS2_PLACEMENT_3D ( 'NONE', #495, #9175, #13957 ) ;
#15773 = LINE ( 'NONE', #15874, #15467 ) ;
#15774 = CARTESIAN_POINT ( 'NONE',  ( -81.02178482187500208, -33.70312499938548711, 102.3871387122750889 ) ) ;
#15775 = CARTESIAN_POINT ( 'NONE',  ( -81.02178482187500208, -33.10312499938548569, -102.3871387122750889 ) ) ;
#15776 = CARTESIAN_POINT ( 'NONE',  ( 81.02178482187500208, -32.54062499938548569, 102.3871387122750889 ) ) ;
#15777 = CARTESIAN_POINT ( 'NONE',  ( 81.02178482187500208, -33.70312499938548711, -102.3871387122750889 ) ) ;
#15778 = CARTESIAN_POINT ( 'NONE',  ( 231.2217848218749339, -32.31562499938547717, -47.61286128772501769 ) ) ;
#15779 = CARTESIAN_POINT ( 'NONE',  ( -79.64356964374999848, -33.06562499938548427, 99.99999999999998579 ) ) ;
#15780 = CARTESIAN_POINT ( 'NONE',  ( 79.64356964374999848, -31.26562499938548356, -99.99999999999998579 ) ) ;
#15781 = VERTEX_POINT ( 'NONE', #14374 ) ;
#15782 = CARTESIAN_POINT ( 'NONE',  ( 79.64356964374999848, -34.97812499938548569, 99.99999999999998579 ) ) ;
#15783 = CARTESIAN_POINT ( 'NONE',  ( 2.807080416178989513, -3.225969019225150003, -3.502507215260505014 ) ) ;
#15784 = CARTESIAN_POINT ( 'NONE',  ( -85.40000000000000568, -32.70000000000000284, 99.99999999999998579 ) ) ;
#15785 = UNCERTAINTY_MEASURE_WITH_UNIT (LENGTH_MEASURE( 1.000000000000000082E-05 ), #16137, 'distance_accuracy_value', 'NONE');
#15786 = VECTOR ( 'NONE', #452, 1000.000000000000000 ) ;
#15787 = CARTESIAN_POINT ( 'NONE',  ( 99.99999999999994316, -29.80000000000000782, -150.0000000000000000 ) ) ;
#15788 = CARTESIAN_POINT ( 'NONE',  ( -81.02178482187500208, -30.29062499938548569, 97.61286128772489690 ) ) ;
#15789 = CARTESIAN_POINT ( 'NONE',  ( 244.7999999999999545, -29.80000000000000426, 150.0000000000000000 ) ) ;
#15790 = EDGE_LOOP ( 'NONE', ( #10156, #17617 ) ) ;
#15791 = CARTESIAN_POINT ( 'NONE',  ( -82.39999999999999147, -34.16250000000000142, -103.4641016151377499 ) ) ;
#15792 = EDGE_CURVE ( 'NONE', #5767, #11694, #3047, .T. ) ;
#15793 = CARTESIAN_POINT ( 'NONE',  ( 82.39999999999999147, -32.81250000000000000, -97.00000000000000000 ) ) ;
#15794 = CARTESIAN_POINT ( 'NONE',  ( 231.0999999999999375, -33.97500000000000142, -47.40192378864679768 ) ) ;
#15795 = CARTESIAN_POINT ( 'NONE',  ( -85.40000000000000568, -29.97441297385334025, 100.9999487804559664 ) ) ;
#15796 = PRESENTATION_LAYER_ASSIGNMENT (  '', '', ( #6133 ) ) ;
#15797 = DIRECTION ( 'NONE',  ( 0.000000000000000000, 0.000000000000000000, 1.000000000000000000 ) ) ;
#15798 = CARTESIAN_POINT ( 'NONE',  ( 82.40000000000001990, -33.88124999877096855, -103.0000000000000000 ) ) ;
#15799 = LINE ( 'NONE', #12662, #16639 ) ;
#15800 = CARTESIAN_POINT ( 'NONE',  ( -80.90000000000000568, -32.34374999877096712, -102.5980762113533018 ) ) ;
#15801 = CARTESIAN_POINT ( 'NONE',  ( 79.64356964374999848, -31.37812499938548427, 99.99999999999998579 ) ) ;
#15802 = VECTOR ( 'NONE', #5775, 1000.000000000000000 ) ;
#15803 = DIRECTION ( 'NONE',  ( -1.387778780781445676E-15, -1.000000000000000000, -0.000000000000000000 ) ) ;
#15804 = DIRECTION ( 'NONE',  ( -0.000000000000000000, -1.000000000000000000, -0.000000000000000000 ) ) ;
#15805 = CARTESIAN_POINT ( 'NONE',  ( 79.64356964375001269, -34.56562499938549138, -101.5914258081833879 ) ) ;
#15806 = DIRECTION ( 'NONE',  ( -0.000000000000000000, -1.000000000000000000, -0.000000000000000000 ) ) ;
#15807 = EDGE_CURVE ( 'NONE', #16790, #893, #14584, .T. ) ;
#15808 = EDGE_LOOP ( 'NONE', ( #15477, #9307, #7448, #15224 ) ) ;
#15809 = CARTESIAN_POINT ( 'NONE',  ( 229.8435696437499587, -34.79062499938547859, -51.59142580818350154 ) ) ;
#15810 = CARTESIAN_POINT ( 'NONE',  ( 231.2217848218749339, -34.22812499938548569, 102.3871387122750889 ) ) ;
#15811 = CARTESIAN_POINT ( 'NONE',  ( 231.2217848218749339, -32.87812499938547717, -47.61286128772501769 ) ) ;
#15812 = CARTESIAN_POINT ( 'NONE',  ( -81.02178482187500208, -30.40312499938548640, 97.61286128772489690 ) ) ;
#15813 = DIRECTION ( 'NONE',  ( 0.000000000000000000, 0.000000000000000000, -1.000000000000000000 ) ) ;
#15814 = ORIENTED_EDGE ( 'NONE', *, *, #9832, .F. ) ;
#15815 = CARTESIAN_POINT ( 'NONE',  ( -79.64356964374999848, -31.26562499938548356, -99.99999999999998579 ) ) ;
#15816 = CARTESIAN_POINT ( 'NONE',  ( 105.1999999999999886, -4.999999999999993783, -103.0000000000000995 ) ) ;
#15817 = EDGE_CURVE ( 'NONE', #10474, #13089, #16710, .T. ) ;
#15818 = VERTEX_POINT ( 'NONE', #4218 ) ;
#15819 = CARTESIAN_POINT ( 'NONE',  ( 79.64356964374999848, -33.62812499938548427, 99.99999999999998579 ) ) ;
#15820 = CARTESIAN_POINT ( 'NONE',  ( -79.64356964374999848, -31.82812499938548356, -99.99999999999998579 ) ) ;
#15821 = CARTESIAN_POINT ( 'NONE',  ( -82.40000000000000568, -34.61250000000001137, 97.00000000000000000 ) ) ;
#15822 = CARTESIAN_POINT ( 'NONE',  ( -79.39999999999999147, -34.63124999877096855, 98.26794919243110371 ) ) ;
#15823 = CIRCLE ( 'NONE', #7713, 7.000000000000006217 ) ;
#15824 = CARTESIAN_POINT ( 'NONE',  ( -79.64356964374999848, -30.47812499938548569, 99.99999999999998579 ) ) ;
#15825 = CARTESIAN_POINT ( 'NONE',  ( -85.15643035625001289, -32.42812499938548854, -101.5914258081833879 ) ) ;
#15826 = CARTESIAN_POINT ( 'NONE',  ( -79.39999999999999147, -34.21874999877096712, -99.99999999999998579 ) ) ;
#15827 = CARTESIAN_POINT ( 'NONE',  ( 231.4702054326072016, -32.00000000000000711, 102.5803447510189699 ) ) ;
#15828 = AXIS2_PLACEMENT_3D ( 'NONE', #5157, #15511, #14132 ) ;
#15829 = CARTESIAN_POINT ( 'NONE',  ( 232.5999999999999375, -31.23749999999999361, 103.4641016151377499 ) ) ;
#15830 = EDGE_CURVE ( 'NONE', #18941, #6967, #3983, .T. ) ;
#15831 = ORIENTED_EDGE ( 'NONE', *, *, #15355, .T. ) ;
#15832 = CARTESIAN_POINT ( 'NONE',  ( 81.02178482187500208, -33.89062499938548711, -97.61286128772489690 ) ) ;
#15833 = CARTESIAN_POINT ( 'NONE',  ( 232.5999999999999375, -32.98124999877096286, 103.4641016151377499 ) ) ;
#15834 = CARTESIAN_POINT ( 'NONE',  ( 229.5999999999999375, -30.84374999877096357, -50.00000000000011369 ) ) ;
#15835 = EDGE_LOOP ( 'NONE', ( #13281, #17177, #11464, #12647 ) ) ;
#15836 = CARTESIAN_POINT ( 'NONE',  ( -82.65380294351676582, -34.99990492518305274, 97.01075526832239859 ) ) ;
#15837 = CARTESIAN_POINT ( 'NONE',  ( -83.77821517812500929, -31.56562499938548427, 97.61286128772489690 ) ) ;
#15838 = VECTOR ( 'NONE', #11837, 1000.000000000000000 ) ;
#15839 = CARTESIAN_POINT ( 'NONE',  ( 109.9999999999999432, -29.80000000000002558, -150.0000000000000000 ) ) ;
#15840 = ORIENTED_EDGE ( 'NONE', *, *, #10457, .T. ) ;
#15841 = CARTESIAN_POINT ( 'NONE',  ( 3.958484000407248793, -2.327740518748946386, 2.968235154690090472 ) ) ;
#15842 = CARTESIAN_POINT ( 'NONE',  ( 232.5999999999999375, -32.00000000000000000, -50.00000000000011369 ) ) ;
#15843 = EDGE_LOOP ( 'NONE', ( #2345, #12878, #2201, #5726 ) ) ;
#15844 = FILL_AREA_STYLE_COLOUR ( '', #6098 ) ;
#15845 = CARTESIAN_POINT ( 'NONE',  ( 79.39999999999999147, -33.37500000000000000, -99.99999999999998579 ) ) ;
#15846 = LINE ( 'NONE', #19161, #15802 ) ;
#15847 = AXIS2_PLACEMENT_3D ( 'NONE', #12387, #4977, #10918 ) ;
#15848 = COLOUR_RGB ( '',0.8941176470588234615, 0.8941176470588234615, 0.8941176470588234615 ) ;
#15849 = CARTESIAN_POINT ( 'NONE',  ( -85.15643035624999868, -31.64062499938548356, 98.40857419181659793 ) ) ;
#15850 = CARTESIAN_POINT ( 'NONE',  ( -80.90000000000000568, -34.34606250001230165, 102.5980762113533018 ) ) ;
#15851 = ADVANCED_FACE ( 'NONE', ( #13293 ), #2750, .F. ) ;
#15852 = CARTESIAN_POINT ( 'NONE',  ( 235.3995413886006247, -34.99999999999998579, -50.31174157908983346 ) ) ;
#15853 = FILL_AREA_STYLE ('',( #14369 ) ) ;
#15854 = CARTESIAN_POINT ( 'NONE',  ( 244.7999999999999545, -32.00000000000002842, 147.7999999999999829 ) ) ;
#15855 = CIRCLE ( 'NONE', #17724, 5.371010071662833063 ) ;
#15856 = CARTESIAN_POINT ( 'NONE',  ( 79.39999999999999147, -33.86250000000000426, 98.26794919243113213 ) ) ;
#15857 = CARTESIAN_POINT ( 'NONE',  ( 0.3126073911696428675, 4.041451884327382338, -3.240528425403984455E-16 ) ) ;
#15858 = CARTESIAN_POINT ( 'NONE',  ( 82.40000000000000568, -34.10624999877096997, -96.99999999999998579 ) ) ;
#15859 = ORIENTED_EDGE ( 'NONE', *, *, #9014, .T. ) ;
#15860 = CARTESIAN_POINT ( 'NONE',  ( 232.8256241621687366, -34.99999999999999289, 97.01974242045224628 ) ) ;
#15861 = PRODUCT_DEFINITION ( 'UNKNOWN', '', #14249, #15291 ) ;
#15862 = CARTESIAN_POINT ( 'NONE',  ( 111.5000000000000142, 12.69999999999998508, 112.0000000000000142 ) ) ;
#15863 = CARTESIAN_POINT ( 'NONE',  ( 235.3564303562499447, -33.66562499938548569, 101.5914258081833879 ) ) ;
#15864 = CARTESIAN_POINT ( 'NONE',  ( -85.15643035624999868, -34.26562499938548711, 101.5914258081833879 ) ) ;
#15865 = CARTESIAN_POINT ( 'NONE',  ( 233.9782151781249411, -30.89062499938548001, -47.61286128772501769 ) ) ;
#15866 = ORIENTED_EDGE ( 'NONE', *, *, #17045, .T. ) ;
#15867 = LINE ( 'NONE', #14647, #4763 ) ;
#15868 = AXIS2_PLACEMENT_3D ( 'NONE', #3383, #3961, #11486 ) ;
#15869 = CARTESIAN_POINT ( 'NONE',  ( -79.64356964374999848, -33.96562499938548285, 99.99999999999998579 ) ) ;
#15870 = LINE ( 'NONE', #19087, #15056 ) ;
#15871 = CARTESIAN_POINT ( 'NONE',  ( 79.39999999999999147, -30.71250000000000568, 98.26794919243113213 ) ) ;
#15872 = CARTESIAN_POINT ( 'NONE',  ( -85.40000000000000568, -32.66250000000000142, 101.7320508075688821 ) ) ;
#15873 = CIRCLE ( 'NONE', #18373, 3.500000000000000000 ) ;
#15874 = CARTESIAN_POINT ( 'NONE',  ( 102.9999999999999858, -5.200000000000008171, -100.0000000000000000 ) ) ;
#15875 = CARTESIAN_POINT ( 'NONE',  ( -85.15643035625001289, -34.75312499938548427, 99.99999999999998579 ) ) ;
#15876 = CARTESIAN_POINT ( 'NONE',  ( -82.39999999999999147, -33.29062499938548569, -96.81714838363319586 ) ) ;
#15877 = CARTESIAN_POINT ( 'NONE',  ( 85.15643035624999868, -31.45312499938548356, 98.40857419181659793 ) ) ;
#15878 = CARTESIAN_POINT ( 'NONE',  ( 79.64356964374999848, -34.07812499938548711, -99.99999999999998579 ) ) ;
#15879 = CARTESIAN_POINT ( 'NONE',  ( 232.5999999999999375, -32.27812499938547575, -46.81714838363331666 ) ) ;
#15880 = CARTESIAN_POINT ( 'NONE',  ( -83.77821517812500929, -32.46562499938548285, 97.61286128772489690 ) ) ;
#15881 = CARTESIAN_POINT ( 'NONE',  ( 83.77821517812500929, -31.56562499938548427, -97.61286128772489690 ) ) ;
#15882 = VERTEX_POINT ( 'NONE', #5782 ) ;
#15883 = CARTESIAN_POINT ( 'NONE',  ( 83.77821517812500929, -34.22812499938549280, 97.61286128772489690 ) ) ;
#15884 = DIRECTION ( 'NONE',  ( 1.000000000000000000, 0.000000000000000000, 0.000000000000000000 ) ) ;
#15885 = CARTESIAN_POINT ( 'NONE',  ( -79.39999999999999147, -32.51250000000000284, 101.7320508075688537 ) ) ;
#15886 = CARTESIAN_POINT ( 'NONE',  ( -81.02178482187500208, -32.54062499938548569, 97.61286128772489690 ) ) ;
#15887 = CARTESIAN_POINT ( 'NONE',  ( -81.02178482187500208, -30.89062499938548711, 102.3871387122750889 ) ) ;
#15888 = CARTESIAN_POINT ( 'NONE',  ( -82.40000000000000568, -30.00000000000000355, 96.99999999999998579 ) ) ;
#15889 = CARTESIAN_POINT ( 'NONE',  ( 105.1999999999999886, -29.80000000000001492, -97.80000000000002558 ) ) ;
#15890 = CARTESIAN_POINT ( 'NONE',  ( -85.40000000000000568, -30.85856250001229029, 101.7320508075688679 ) ) ;
#15891 = CARTESIAN_POINT ( 'NONE',  ( 4.086376042167605860, 1.979461949354204719, -3.571471332069179105 ) ) ;
#15892 = CARTESIAN_POINT ( 'NONE',  ( -79.39999999999999147, -32.90624999877096712, 101.7320508075688537 ) ) ;
#15893 = DIRECTION ( 'NONE',  ( 0.8660254037844374864, -0.5000000000000018874, 0.000000000000000000 ) ) ;
#15894 = DIRECTION ( 'NONE',  ( -0.000000000000000000, -1.000000000000000000, -0.000000000000000000 ) ) ;
#15895 = ADVANCED_FACE ( 'NONE', ( #4411 ), #6103, .F. ) ;
#15896 = CARTESIAN_POINT ( 'NONE',  ( 234.9223452063436355, -31.99999999999999289, 98.15128725331840087 ) ) ;
#15897 = DIRECTION ( 'NONE',  ( -1.000000000000000000, -0.000000000000000000, -0.000000000000000000 ) ) ;
#15898 = CARTESIAN_POINT ( 'NONE',  ( 79.64356964374999848, -34.97812499938548569, -99.99999999999998579 ) ) ;
#15899 = CARTESIAN_POINT ( 'NONE',  ( 4.142654963991902584, 2.035398498734314554, 3.525413613457253792 ) ) ;
#15900 = VERTEX_POINT ( 'NONE', #12576 ) ;
#15901 =( BOUNDED_CURVE ( )  B_SPLINE_CURVE ( 2, ( #1572, #1664, #6065, #12011, #6448, #4594, #10932, #10552, #12399 ),
 .UNSPECIFIED., .F., .F. ) 
 B_SPLINE_CURVE_WITH_KNOTS ( ( 3, 2, 2, 2, 3 ),
 ( 0.6458333333333332593, 0.6527777777777777901, 0.6666666666666666297, 0.6805555555555555802, 0.6875000000000000000 ),
 .UNSPECIFIED. ) 
 CURVE ( )  GEOMETRIC_REPRESENTATION_ITEM ( )  RATIONAL_B_SPLINE_CURVE ( ( 0.9330127018922192983, 0.9330127018922187432, 1.000000000000000000, 0.8660254037844387076, 1.000000000000000000, 0.8660254037844387076, 1.000000000000000000, 0.9330127018922194093, 0.9330127018922194093 ) ) 
 REPRESENTATION_ITEM ( '' )  );
#15902 = CARTESIAN_POINT ( 'NONE',  ( 79.39999999999999147, -32.45624999877097139, 98.26794919243113213 ) ) ;
#15903 = ITEM_DEFINED_TRANSFORMATION ( 'NONE', 'NONE', #2068,  #10540 ) ;
#15904 = CARTESIAN_POINT ( 'NONE',  ( 229.8435696437499871, -34.26562499938548001, 101.5914258081833879 ) ) ;
#15905 = CARTESIAN_POINT ( 'NONE',  ( 233.9782151781249411, -33.10312499938547859, -52.38713871227520968 ) ) ;
#15906 = CARTESIAN_POINT ( 'NONE',  ( -79.77811200999887831, -35.00000000000000000, 100.8506536761481414 ) ) ;
#15907 = PLANE ( 'NONE',  #5570 ) ;
#15908 = ORIENTED_EDGE ( 'NONE', *, *, #18718, .T. ) ;
#15909 = CARTESIAN_POINT ( 'NONE',  ( -83.77821517812500929, -32.91562499938547859, -102.3871387122750889 ) ) ;
#15910 = CARTESIAN_POINT ( 'NONE',  ( -94.79999999999999716, -3.000000000000000000, -150.0000000000000000 ) ) ;
#15911 = ORIENTED_EDGE ( 'NONE', *, *, #3153, .T. ) ;
#15912 = CARTESIAN_POINT ( 'NONE',  ( 83.77821517812500929, -34.22812499938549280, 97.61286128772489690 ) ) ;
#15913 = CARTESIAN_POINT ( 'NONE',  ( -85.15643035625001289, -31.15312499938548996, -99.99999999999998579 ) ) ;
#15914 = CARTESIAN_POINT ( 'NONE',  ( 85.40000000000000568, -33.56250000000000000, 98.26794919243111792 ) ) ;
#15915 = CARTESIAN_POINT ( 'NONE',  ( -79.59365286754820090, -34.99999999999999289, 99.92898555286045337 ) ) ;
#15916 = CARTESIAN_POINT ( 'NONE',  ( -79.39999999999999147, -35.15624999877096712, 101.7320508075688537 ) ) ;
#15917 = CARTESIAN_POINT ( 'NONE',  ( -79.64356964375001269, -31.86562499938548143, 101.5914258081833879 ) ) ;
#15918 = CARTESIAN_POINT ( 'NONE',  ( -82.39999999999999147, -33.85312499938548569, -103.1828516163667899 ) ) ;
#15919 = EDGE_CURVE ( 'NONE', #518, #4595, #11463, .T. ) ;
#15920 = PRODUCT_DEFINITION_SHAPE ( 'NONE', 'NONE',  #18016 ) ;
#15921 = LINE ( 'NONE', #17676, #276 ) ;
#15922 = CARTESIAN_POINT ( 'NONE',  ( 85.40000000000000568, -31.33124999877096428, -98.26794919243111792 ) ) ;
#15923 = CARTESIAN_POINT ( 'NONE',  ( 231.0999999999999375, -31.87499999999999289, 97.40192378864668399 ) ) ;
#15924 = ADVANCED_FACE ( 'NONE', ( #676 ), #1836, .F. ) ;
#15925 = ORIENTED_EDGE ( 'NONE', *, *, #10908, .T. ) ;
#15926 = CARTESIAN_POINT ( 'NONE',  ( 235.5999999999999375, -34.66874999877096286, 99.99999999999998579 ) ) ;
#15927 = CARTESIAN_POINT ( 'NONE',  ( 234.0999999999999375, -32.04374999877096286, 102.5980762113533018 ) ) ;
#15928 = CARTESIAN_POINT ( 'NONE',  ( 229.5999999999999375, -31.25624999877096144, -48.26794919243123161 ) ) ;
#15929 = DIRECTION ( 'NONE',  ( 0.000000000000000000, -0.8660254037844380415, 0.5000000000000012212 ) ) ;
#15930 = EDGE_LOOP ( 'NONE', ( #16900, #12609, #12995, #2780 ) ) ;
#15931 = VERTEX_POINT ( 'NONE', #9255 ) ;
#15932 = CARTESIAN_POINT ( 'NONE',  ( 4.180345304246197990, -2.049116244671344234, 3.591763845239310804 ) ) ;
#15933 = CARTESIAN_POINT ( 'NONE',  ( 4.175075985190095373, -2.060370777630105454, 3.568666869285574084 ) ) ;
#15934 = EDGE_LOOP ( 'NONE', ( #6558, #17328, #6734, #6443, #18582 ) ) ;
#15935 =( BOUNDED_CURVE ( )  B_SPLINE_CURVE ( 2, ( #6817, #12468, #12763, #15502, #3964 ),
 .UNSPECIFIED., .F., .F. ) 
 B_SPLINE_CURVE_WITH_KNOTS ( ( 3, 2, 3 ),
 ( 0.000000000000000000, 0.01388888888888888812, 0.02083333333333332871 ),
 .UNSPECIFIED. ) 
 CURVE ( )  GEOMETRIC_REPRESENTATION_ITEM ( )  RATIONAL_B_SPLINE_CURVE ( ( 1.000000000000000000, 0.8660254037844387076, 1.000000000000000000, 0.9330127018922194093, 0.9330127018922191873 ) ) 
 REPRESENTATION_ITEM ( '' )  );
#15936 = DIRECTION ( 'NONE',  ( -0.000000000000000000, -0.000000000000000000, -1.000000000000000000 ) ) ;
#15937 = CARTESIAN_POINT ( 'NONE',  ( 80.90000000000000568, -32.85000000000000142, -97.40192378864668399 ) ) ;
#15938 = CARTESIAN_POINT ( 'NONE',  ( 82.86160995759659897, -32.00000000000000000, -102.8104067583495578 ) ) ;
#15939 = EDGE_CURVE ( 'NONE', #8256, #10239, #16689, .T. ) ;
#15940 = CARTESIAN_POINT ( 'NONE',  ( -79.64356964374999848, -31.82812499938548356, 99.99999999999998579 ) ) ;
#15941 = CARTESIAN_POINT ( 'NONE',  ( -80.90000000000000568, -31.94999999999999929, 97.40192378864668399 ) ) ;
#15942 = CARTESIAN_POINT ( 'NONE',  ( 4.197393957002303999, 7.772902908466098641E-14, -3.503767560748929810 ) ) ;
#15943 =( NAMED_UNIT ( * ) SI_UNIT ( $, .STERADIAN. ) SOLID_ANGLE_UNIT ( ) );
#15944 = ADVANCED_FACE ( 'NONE', ( #12480 ), #18543, .F. ) ;
#15945 = CARTESIAN_POINT ( 'NONE',  ( 232.5999999999999375, -32.30624999877096570, -53.00000000000011369 ) ) ;
#15946 = CARTESIAN_POINT ( 'NONE',  ( 0.000000000000000000, 0.000000000000000000, -4.000000000000000000 ) ) ;
#15947 = CARTESIAN_POINT ( 'NONE',  ( -85.15643035624999868, -35.05312499938548143, 101.5914258081833879 ) ) ;
#15948 = FACE_OUTER_BOUND ( 'NONE', #10074, .T. ) ;
#15949 = VERTEX_POINT ( 'NONE', #2024 ) ;
#15950 = CARTESIAN_POINT ( 'NONE',  ( 229.5999999999999375, -34.04999999999999716, -50.00000000000011369 ) ) ;
#15951 = CARTESIAN_POINT ( 'NONE',  ( -84.51154815724953551, -35.25364861271051353, -101.7717992799616553 ) ) ;
#15952 = DIRECTION ( 'NONE',  ( -0.000000000000000000, -1.000000000000000000, -0.000000000000000000 ) ) ;
#15953 = CARTESIAN_POINT ( 'NONE',  ( -82.39999999999999147, -34.83749999999999858, -97.00000000000000000 ) ) ;
#15954 = CARTESIAN_POINT ( 'NONE',  ( -85.15643035624999868, -33.36562499938548854, 101.5914258081833879 ) ) ;
#15955 = CARTESIAN_POINT ( 'NONE',  ( 235.3564303562499447, -34.52812499938547575, -50.00000000000011369 ) ) ;
#15956 = VERTEX_POINT ( 'NONE', #15221 ) ;
#15957 = CARTESIAN_POINT ( 'NONE',  ( -83.77821517812500929, -33.66562499938548569, 102.3871387122750889 ) ) ;
#15958 = CARTESIAN_POINT ( 'NONE',  ( -82.39999999999999147, -30.50624999877097210, 96.53589838486223584 ) ) ;
#15959 = CARTESIAN_POINT ( 'NONE',  ( 85.15643035625001289, -35.09062499938548285, 99.99999999999998579 ) ) ;
#15960 = LINE ( 'NONE', #2566, #1201 ) ;
#15961 = CARTESIAN_POINT ( 'NONE',  ( 229.8435696437499871, -32.35312499938547859, 101.5914258081833879 ) ) ;
#15962 = CARTESIAN_POINT ( 'NONE',  ( 235.3564303562499447, -32.20312499938548001, -48.40857419181671162 ) ) ;
#15963 = EDGE_CURVE ( 'NONE', #18433, #2579, #8184, .T. ) ;
#15964 = CARTESIAN_POINT ( 'NONE',  ( -79.64356964374998427, -33.21562499938548996, 101.5914258081833879 ) ) ;
#15965 = CARTESIAN_POINT ( 'NONE',  ( -83.77821517812500929, -33.47812499938548569, -102.3871387122750889 ) ) ;
#15966 = CARTESIAN_POINT ( 'NONE',  ( 83.90000000000000568, -33.16874999877096286, -97.40192378864668399 ) ) ;
#15967 =( BOUNDED_CURVE ( )  B_SPLINE_CURVE ( 2, ( #10307, #16265, #9028, #6005, #11671, #2970, #14689, #1612, #16173 ),
 .UNSPECIFIED., .F., .F. ) 
 B_SPLINE_CURVE_WITH_KNOTS ( ( 3, 2, 2, 2, 3 ),
 ( 0.8125000000000001110, 0.8194444444444444198, 0.8333333333333333703, 0.8472222222222222099, 0.8530683953269213582 ),
 .UNSPECIFIED. ) 
 CURVE ( )  GEOMETRIC_REPRESENTATION_ITEM ( )  RATIONAL_B_SPLINE_CURVE ( ( 0.9330127018922194093, 0.9330127018922204085, 1.000000000000000000, 0.8660254037844387076, 1.000000000000000000, 0.8660254037844387076, 1.000000000000000000, 0.9436068149601996025, 0.9346881722405915305 ) ) 
 REPRESENTATION_ITEM ( '' )  );
#15968 = B_SPLINE_CURVE_WITH_KNOTS ( 'NONE', 3,
 ( #17016, #5108, #15455, #12232, #5014, #10954, #9389, #15354, #16831, #3438, #18201, #13592, #9196, #15260, #232, #4914, #6285, #621 ),
 .UNSPECIFIED., .F., .F.,
 ( 4, 2, 2, 2, 2, 2, 2, 2, 4 ),
 ( 0.000000000000000000, 0.0007106627595359156415, 0.001421325519071831283, 0.002131988278607746708, 0.002842651038143662566, 0.003553313797679578424, 0.004263976557215493415, 0.004974639316751409274, 0.005685302076287325132 ),
 .UNSPECIFIED. ) ;
#15969 = CARTESIAN_POINT ( 'NONE',  ( 82.39999999999999147, -35.09062499938548285, -103.1828516163667899 ) ) ;
#15970 = CARTESIAN_POINT ( 'NONE',  ( 235.3564303562499447, -33.55312499938548143, -48.40857419181671162 ) ) ;
#15971 = CARTESIAN_POINT ( 'NONE',  ( -85.15643035625001289, -33.70312499938548711, 101.5914258081833879 ) ) ;
#15972 = CARTESIAN_POINT ( 'NONE',  ( 83.77821517812500929, -30.96562499938548640, -102.3871387122750889 ) ) ;
#15973 = EDGE_LOOP ( 'NONE', ( #6326, #6467, #10575, #7183 ) ) ;
#15974 = CARTESIAN_POINT ( 'NONE',  ( 83.77821517812500929, -35.12812499938548427, 97.61286128772489690 ) ) ;
#15975 = CARTESIAN_POINT ( 'NONE',  ( 232.5999999999999375, -29.99999999999999645, 103.0000000000000000 ) ) ;
#15976 = ADVANCED_FACE ( 'NONE', ( #3298 ), #14270, .T. ) ;
#15977 = PRODUCT_DEFINITION ( 'UNKNOWN', '', #1152, #10948 ) ;
#15978 = CARTESIAN_POINT ( 'NONE',  ( -79.39999999999999147, -32.43750000000000000, 98.26794919243110371 ) ) ;
#15979 = CARTESIAN_POINT ( 'NONE',  ( -85.15643035624999868, -34.15312499938548285, 101.5914258081833879 ) ) ;
#15980 = CARTESIAN_POINT ( 'NONE',  ( -85.15643035625001289, -31.04062499938548569, 99.99999999999998579 ) ) ;
#15981 = ORIENTED_EDGE ( 'NONE', *, *, #6542, .T. ) ;
#15982 = CARTESIAN_POINT ( 'NONE',  ( -85.40000000000000568, -31.35000000000000142, 99.99999999999998579 ) ) ;
#15983 = AXIS2_PLACEMENT_3D ( 'NONE', #10356, #14547, #8699 ) ;
#15984 = CYLINDRICAL_SURFACE ( 'NONE', #12855, 3.000000000000002665 ) ;
#15985 = FACE_OUTER_BOUND ( 'NONE', #5693, .T. ) ;
#15986 = CYLINDRICAL_SURFACE ( 'NONE', #9216, 3.000000000000002665 ) ;
#15987 = CARTESIAN_POINT ( 'NONE',  ( -84.42750213138106119, -35.00000000000000711, 97.77995849557629526 ) ) ;
#15988 = DIRECTION ( 'NONE',  ( 0.000000000000000000, -1.000000000000000000, 0.000000000000000000 ) ) ;
#15989 = CARTESIAN_POINT ( 'NONE',  ( 84.44763168836732348, -32.00000000000002132, 98.15470523285560489 ) ) ;
#15990 = DIRECTION ( 'NONE',  ( -1.000000000000000000, 0.000000000000000000, 0.000000000000000000 ) ) ;
#15991 = CARTESIAN_POINT ( 'NONE',  ( -4.000000000000000000, -2.309401076758512694, -3.433295621305382461 ) ) ;
#15992 = CARTESIAN_POINT ( 'NONE',  ( -82.39999999999999147, -32.58749999999999858, -96.99999999999998579 ) ) ;
#15993 = CARTESIAN_POINT ( 'NONE',  ( 81.02178482187500208, -34.15312499938548285, -102.3871387122750889 ) ) ;
#15994 = CARTESIAN_POINT ( 'NONE',  ( 111.5000000000000142, 12.69999999999998508, 50.00000000000001421 ) ) ;
#15995 = VECTOR ( 'NONE', #3923, 1000.000000000000000 ) ;
#15996 = VECTOR ( 'NONE', #6990, 1000.000000000000000 ) ;
#15997 = ORIENTED_EDGE ( 'NONE', *, *, #15335, .T. ) ;
#15998 = CARTESIAN_POINT ( 'NONE',  ( 79.39999999999999147, -32.00624999877096855, 98.26794919243113213 ) ) ;
#15999 = CARTESIAN_POINT ( 'NONE',  ( 235.3564303562499447, -34.07812499938548001, 99.99999999999998579 ) ) ;
#16000 = CARTESIAN_POINT ( 'NONE',  ( 229.8435696437499871, -33.81562499938547717, -48.40857419181671162 ) ) ;
#16001 = LINE ( 'NONE', #5562, #13654 ) ;
#16002 = CARTESIAN_POINT ( 'NONE',  ( 85.40000000000000568, -34.08749999999999858, 101.7320508075688821 ) ) ;
#16003 = ORIENTED_EDGE ( 'NONE', *, *, #13908, .T. ) ;
#16004 = CARTESIAN_POINT ( 'NONE',  ( -79.64356964375001269, -34.00312499938549138, -98.40857419181659793 ) ) ;
#16005 = CARTESIAN_POINT ( 'NONE',  ( -85.40000000000000568, -30.00000000000000355, 99.99999999999998579 ) ) ;
#16006 = VERTEX_POINT ( 'NONE', #15314 ) ;
#16007 = CARTESIAN_POINT ( 'NONE',  ( -83.20384757729337366, -34.80134618820331127, -97.00000000000000000 ) ) ;
#16008 = CARTESIAN_POINT ( 'NONE',  ( -85.15643035624999868, -32.09062499938548996, -101.5914258081833879 ) ) ;
#16009 = AXIS2_PLACEMENT_3D ( 'NONE', #9250, #11003, #10814 ) ;
#16010 = CARTESIAN_POINT ( 'NONE',  ( 80.90000000000000568, -34.80000000000000426, 97.40192378864668399 ) ) ;
#16011 = CARTESIAN_POINT ( 'NONE',  ( 232.5999999999999375, -30.59062499938547930, 103.1828516163667899 ) ) ;
#16012 = CARTESIAN_POINT ( 'NONE',  ( -79.39999999999999147, -35.08124999877097139, 98.26794919243110371 ) ) ;
#16013 = B_SPLINE_CURVE_WITH_KNOTS ( 'NONE', 1,
 ( #3790, #16005 ),
 .UNSPECIFIED., .F., .F.,
 ( 2, 2 ),
 ( 0.000000000000000000, 1.000000000000000000 ),
 .UNSPECIFIED. ) ;
#16014 = CARTESIAN_POINT ( 'NONE',  ( -82.39999999999999147, -31.26562499938549067, 96.81714838363319586 ) ) ;
#16015 = CARTESIAN_POINT ( 'NONE',  ( -82.39999999999999147, -33.40312499938548285, -103.1828516163667899 ) ) ;
#16016 =( BOUNDED_CURVE ( )  B_SPLINE_CURVE ( 3, ( #14543, #8309, #9779, #17496 ),
 .UNSPECIFIED., .F., .F. ) 
 B_SPLINE_CURVE_WITH_KNOTS ( ( 4, 4 ),
 ( 1.531555772456618891, 1.570796326794896780 ),
 .UNSPECIFIED. ) 
 CURVE ( )  GEOMETRIC_REPRESENTATION_ITEM ( )  RATIONAL_B_SPLINE_CURVE ( ( 1.000000000000000000, 0.9998716856909537487, 0.9998716856909537487, 1.000000000000000000 ) ) 
 REPRESENTATION_ITEM ( '' )  );
#16017 = CARTESIAN_POINT ( 'NONE',  ( 232.5999999999999375, -29.99999999999999645, 99.99999999999998579 ) ) ;
#16018 = CARTESIAN_POINT ( 'NONE',  ( 79.39999999999999147, -31.48124999877097352, -98.26794919243110371 ) ) ;
#16019 = CARTESIAN_POINT ( 'NONE',  ( 234.0999999999999375, -30.29999999999999716, 102.5980762113533018 ) ) ;
#16020 = ORIENTED_EDGE ( 'NONE', *, *, #9427, .F. ) ;
#16021 = CARTESIAN_POINT ( 'NONE',  ( 229.8435696437499587, -32.09062499938548285, -51.59142580818350154 ) ) ;
#16022 =( NAMED_UNIT ( * ) PLANE_ANGLE_UNIT ( ) SI_UNIT ( $, .RADIAN. ) );
#16023 = CARTESIAN_POINT ( 'NONE',  ( 229.5999999999999375, -33.54374999877096286, 99.99999999999998579 ) ) ;
#16024 = DIRECTION ( 'NONE',  ( -1.000000000000000000, 0.000000000000000000, 0.000000000000000000 ) ) ;
#16025 = LINE ( 'NONE', #8589, #6465 ) ;
#16026 = CARTESIAN_POINT ( 'NONE',  ( -83.77821517812500929, -30.66562499938548569, 97.61286128772489690 ) ) ;
#16027 = EDGE_LOOP ( 'NONE', ( #6187, #11289 ) ) ;
#16028 = EDGE_LOOP ( 'NONE', ( #7636, #10270, #509, #18424 ) ) ;
#16029 = CARTESIAN_POINT ( 'NONE',  ( -79.58826230849687988, -32.00000000000094502, 98.95399275615287138 ) ) ;
#16030 = DIRECTION ( 'NONE',  ( -0.000000000000000000, -0.000000000000000000, 1.000000000000000000 ) ) ;
#16031 = ORIENTED_EDGE ( 'NONE', *, *, #10900, .F. ) ;
#16032 = CARTESIAN_POINT ( 'NONE',  ( 85.40000000000000568, -32.70000000000000284, -99.99999999999998579 ) ) ;
#16033 = DIRECTION ( 'NONE',  ( 1.000000000000000000, -0.000000000000000000, -2.407412430484046130E-31 ) ) ;
#16034 = ADVANCED_FACE ( 'NONE', ( #17074 ), #388, .F. ) ;
#16035 = EDGE_CURVE ( 'NONE', #14464, #13696, #2417, .T. ) ;
#16036 = CARTESIAN_POINT ( 'NONE',  ( -85.15643035625001289, -31.60312499938548569, 99.99999999999998579 ) ) ;
#16037 = CARTESIAN_POINT ( 'NONE',  ( -83.90000000000000568, -31.87500000000000000, 97.40192378864668399 ) ) ;
#16038 = CARTESIAN_POINT ( 'NONE',  ( 235.3058334582606506, -35.00000000000002132, -49.37250936986590943 ) ) ;
#16039 = CARTESIAN_POINT ( 'NONE',  ( 79.64356964374999848, -34.52812499938548285, -99.99999999999998579 ) ) ;
#16040 = DIRECTION ( 'NONE',  ( 0.000000000000000000, -1.000000000000000000, 0.000000000000000000 ) ) ;
#16041 = FACE_OUTER_BOUND ( 'NONE', #1245, .T. ) ;
#16042 = CARTESIAN_POINT ( 'NONE',  ( -83.20384757729335945, -34.40759618943233988, -96.99999999999998579 ) ) ;
#16043 = ORIENTED_EDGE ( 'NONE', *, *, #3012, .T. ) ;
#16044 = CARTESIAN_POINT ( 'NONE',  ( -79.64356964374999848, -31.26562499938548356, -99.99999999999998579 ) ) ;
#16045 = DIRECTION ( 'NONE',  ( -0.000000000000000000, -1.000000000000000000, -0.000000000000000000 ) ) ;
#16046 = ADVANCED_FACE ( 'NONE', ( #16787 ), #3400, .F. ) ;
#16047 =( BOUNDED_CURVE ( )  B_SPLINE_CURVE ( 2, ( #14999, #10693, #1620, #16660, #13236, #7572, #6216, #10603, #1335 ),
 .UNSPECIFIED., .F., .F. ) 
 B_SPLINE_CURVE_WITH_KNOTS ( ( 3, 2, 2, 2, 3 ),
 ( 0.5625000000000000000, 0.5694444444444444198, 0.5833333333333333703, 0.5972222222222222099, 0.6041666666666666297 ),
 .UNSPECIFIED. ) 
 CURVE ( )  GEOMETRIC_REPRESENTATION_ITEM ( )  RATIONAL_B_SPLINE_CURVE ( ( 0.9330127018922194093, 0.9330127018922194093, 1.000000000000000000, 0.8660254037844387076, 1.000000000000000000, 0.8660254037844387076, 1.000000000000000000, 0.9330127018922198534, 0.9330127018922192983 ) ) 
 REPRESENTATION_ITEM ( '' )  );
#16048 = CARTESIAN_POINT ( 'NONE',  ( 83.90000000000000568, -34.96874999877096712, 102.5980762113533018 ) ) ;
#16049 = CARTESIAN_POINT ( 'NONE',  ( 0.000000000000000000, 0.000000000000000000, 0.000000000000000000 ) ) ;
#16050 = CARTESIAN_POINT ( 'NONE',  ( -79.64356964375001269, -32.76562499938548711, 101.5914258081833879 ) ) ;
#16051 = CARTESIAN_POINT ( 'NONE',  ( 80.90000000000000568, -32.55000000000000426, 97.40192378864668399 ) ) ;
#16052 = CARTESIAN_POINT ( 'NONE',  ( 231.2217848218749339, -32.76562499938548001, -47.61286128772501769 ) ) ;
#16053 = VERTEX_POINT ( 'NONE', #16885 ) ;
#16054 = CARTESIAN_POINT ( 'NONE',  ( -85.15643035625001289, -33.74062499938548854, 99.99999999999998579 ) ) ;
#16055 = EDGE_CURVE ( 'NONE', #18944, #1594, #10029, .T. ) ;
#16056 = CARTESIAN_POINT ( 'NONE',  ( 246.9999999999999716, -29.80000000000000426, 150.0000000000000000 ) ) ;
#16057 = CARTESIAN_POINT ( 'NONE',  ( 81.02178482187500208, -33.89062499938548711, 102.3871387122750889 ) ) ;
#16058 = CARTESIAN_POINT ( 'NONE',  ( -85.40000000000000568, -32.73750000000000426, 98.26794919243111792 ) ) ;
#16059 = CARTESIAN_POINT ( 'NONE',  ( 233.9782151781249411, -31.19062499938547717, 97.61286128772489690 ) ) ;
#16060 = LINE ( 'NONE', #11566, #7041 ) ;
#16061 = CARTESIAN_POINT ( 'NONE',  ( 5.599999999999999645, 2.020725942163686728, -3.499999999999999556 ) ) ;
#16062 = CARTESIAN_POINT ( 'NONE',  ( -82.39999999999999147, -33.51562499938548711, -103.1828516163667899 ) ) ;
#16063 = PLANE ( 'NONE',  #8374 ) ;
#16064 = CARTESIAN_POINT ( 'NONE',  ( 81.02178482187500208, -33.55312499938548854, -97.61286128772489690 ) ) ;
#16065 = CARTESIAN_POINT ( 'NONE',  ( 234.0999999999999375, -30.59999999999999432, -52.59807621135342970 ) ) ;
#16066 = CARTESIAN_POINT ( 'NONE',  ( -82.39999999999999147, -32.72812499938548569, 103.1828516163667899 ) ) ;
#16067 = CARTESIAN_POINT ( 'NONE',  ( 85.15643035624999868, -30.62812499938548427, -98.40857419181659793 ) ) ;
#16068 = ORIENTED_EDGE ( 'NONE', *, *, #6653, .T. ) ;
#16069 = FACE_OUTER_BOUND ( 'NONE', #11439, .T. ) ;
#16070 = CARTESIAN_POINT ( 'NONE',  ( -0.1404048886732797152, -4.699864953788083888, -3.686887068327043160 ) ) ;
#16071 = CARTESIAN_POINT ( 'NONE',  ( -79.39999999999999147, -33.78750000000000142, 98.26794919243110371 ) ) ;
#16072 = CARTESIAN_POINT ( 'NONE',  ( -85.15643035624999868, -33.25312499938548427, 101.5914258081833879 ) ) ;
#16073 = CARTESIAN_POINT ( 'NONE',  ( -81.02178482187500208, -31.79062499938548925, 102.3871387122750889 ) ) ;
#16074 = ORIENTED_EDGE ( 'NONE', *, *, #11875, .F. ) ;
#16075 = FACE_OUTER_BOUND ( 'NONE', #17301, .T. ) ;
#16076 = AXIS2_PLACEMENT_3D ( 'NONE', #7232, #4403, #8598 ) ;
#16077 = CARTESIAN_POINT ( 'NONE',  ( 235.3564303562499447, -33.10312499938547859, 101.5914258081833879 ) ) ;
#16078 = CARTESIAN_POINT ( 'NONE',  ( 82.17437583783166133, -34.99999999999999289, -97.01974242045223207 ) ) ;
#16079 = DIRECTION ( 'NONE',  ( 0.000000000000000000, 0.000000000000000000, -1.000000000000000000 ) ) ;
#16080 =( BOUNDED_CURVE ( )  B_SPLINE_CURVE ( 2, ( #8164, #14022, #13731, #1908, #18237, #2006, #12274, #657, #370 ),
 .UNSPECIFIED., .F., .F. ) 
 B_SPLINE_CURVE_WITH_KNOTS ( ( 3, 2, 2, 2, 3 ),
 ( 0.7708333333333332593, 0.7777777777777777901, 0.7916666666666666297, 0.8055555555555555802, 0.8125000000000000000 ),
 .UNSPECIFIED. ) 
 CURVE ( )  GEOMETRIC_REPRESENTATION_ITEM ( )  RATIONAL_B_SPLINE_CURVE ( ( 0.9330127018922192983, 0.9330127018922187432, 1.000000000000000000, 0.8660254037844387076, 1.000000000000000000, 0.8660254037844387076, 1.000000000000000000, 0.9330127018922194093, 0.9330127018922194093 ) ) 
 REPRESENTATION_ITEM ( '' )  );
#16081 = CARTESIAN_POINT ( 'NONE',  ( -85.40000000000000568, -34.46249999999999858, 101.7320508075688821 ) ) ;
#16082 = B_SPLINE_CURVE_WITH_KNOTS ( 'NONE', 3,
 ( #2694, #6917, #9938, #2407, #16088, #862, #12866, #8652, #12771, #12959, #2596, #8556, #17363, #3972, #15896, #8274, #2502, #7005 ),
 .UNSPECIFIED., .F., .F.,
 ( 4, 2, 2, 2, 2, 2, 2, 2, 4 ),
 ( 0.000000000000000000, 0.0007089252359835998551, 0.001417850471967199710, 0.002126775707950799565, 0.002835700943934399421, 0.003544626179917999276, 0.004253551415901599131, 0.004962476651885198986, 0.005671401887868798841 ),
 .UNSPECIFIED. ) ;
#16083 = EDGE_CURVE ( 'NONE', #7832, #17884, #10095, .T. ) ;
#16084 = CARTESIAN_POINT ( 'NONE',  ( -79.39999999999999147, -32.83124999877097139, 98.26794919243110371 ) ) ;
#16085 = DIRECTION ( 'NONE',  ( -0.000000000000000000, -1.000000000000000000, -0.000000000000000000 ) ) ;
#16086 = CARTESIAN_POINT ( 'NONE',  ( -82.40000000000000568, -32.30624999877097281, -102.9999999999999858 ) ) ;
#16087 = CARTESIAN_POINT ( 'NONE',  ( 81.02178482187500208, -33.55312499938548854, 102.3871387122750889 ) ) ;
#16088 = CARTESIAN_POINT ( 'NONE',  ( 231.6947747743589616, -31.99999999999999289, 97.33297554273077878 ) ) ;
#16089 = CARTESIAN_POINT ( 'NONE',  ( -83.20384757729337366, -32.79240381056766296, -103.0000000000000000 ) ) ;
#16090 = CARTESIAN_POINT ( 'NONE',  ( 79.64356964375001269, -32.69062499938548427, -98.40857419181659793 ) ) ;
#16091 = CARTESIAN_POINT ( 'NONE',  ( 231.7961524227065695, -33.95759618943232283, 102.9999999999999716 ) ) ;
#16092 = CIRCLE ( 'NONE', #4239, 5.200000000000009948 ) ;
#16093 = ORIENTED_EDGE ( 'NONE', *, *, #9098, .T. ) ;
#16094 = CARTESIAN_POINT ( 'NONE',  ( 85.40000000000000568, -33.50624999877096855, 98.26794919243111792 ) ) ;
#16095 = CONTEXT_DEPENDENT_SHAPE_REPRESENTATION ( #9957, #14346 ) ;
#16096 = CARTESIAN_POINT ( 'NONE',  ( 235.3564303562499447, -34.49062499938548143, 98.40857419181659793 ) ) ;
#16097 = CARTESIAN_POINT ( 'NONE',  ( 231.2217848218749339, -35.12812499938548427, -47.61286128772501769 ) ) ;
#16098 = CARTESIAN_POINT ( 'NONE',  ( 244.7999999999999545, -35.00000000000000000, -100.0000000000000000 ) ) ;
#16099 = DIRECTION ( 'NONE',  ( 0.000000000000000000, 0.000000000000000000, 1.000000000000000000 ) ) ;
#16100 = ORIENTED_EDGE ( 'NONE', *, *, #19145, .T. ) ;
#16101 = CARTESIAN_POINT ( 'NONE',  ( -79.64356964375001269, -34.82812499938548711, -101.5914258081833879 ) ) ;
#16102 = CARTESIAN_POINT ( 'NONE',  ( 79.39999999999999147, -32.45624999877097139, 98.26794919243113213 ) ) ;
#16103 = ORIENTED_EDGE ( 'NONE', *, *, #1604, .F. ) ;
#16104 = EDGE_CURVE ( 'NONE', #5607, #17007, #9984, .T. ) ;
#16105 = CARTESIAN_POINT ( 'NONE',  ( 99.99999999999995737, -21.80000000000003268, -142.6499999999999773 ) ) ;
#16106 = CARTESIAN_POINT ( 'NONE',  ( -81.02178482187500208, -30.85312499938548569, -102.3871387122750889 ) ) ;
#16107 = AXIS2_PLACEMENT_3D ( 'NONE', #9490, #12715, #18689 ) ;
#16108 = CARTESIAN_POINT ( 'NONE',  ( -80.90000000000000568, -32.49374999877097281, -97.40192378864668399 ) ) ;
#16109 = CARTESIAN_POINT ( 'NONE',  ( -81.05805657947830412, -35.00000000000002842, 97.38506107425214964 ) ) ;
#16110 = CARTESIAN_POINT ( 'NONE',  ( -83.90000000000000568, -34.96874999877096712, 97.40192378864668399 ) ) ;
#16111 = CARTESIAN_POINT ( 'NONE',  ( -82.39999999999999147, -30.36562499938549209, 96.81714838363319586 ) ) ;
#16112 = CARTESIAN_POINT ( 'NONE',  ( -79.64356964374998427, -32.65312499938548285, -98.40857419181659793 ) ) ;
#16113 = FACE_OUTER_BOUND ( 'NONE', #12329, .T. ) ;
#16114 = CARTESIAN_POINT ( 'NONE',  ( 79.58826230851033756, -31.99999999999998579, 101.0460072438832952 ) ) ;
#16115 = CARTESIAN_POINT ( 'NONE',  ( 82.39999999999999147, -32.30624999877097281, -96.53589838486223584 ) ) ;
#16116 = CARTESIAN_POINT ( 'NONE',  ( 229.5999999999999375, -30.03749999999999432, 98.26794919243111792 ) ) ;
#16117 = MECHANICAL_DESIGN_GEOMETRIC_PRESENTATION_REPRESENTATION (  '', ( #13965 ), #7366 ) ;
#16118 = VERTEX_POINT ( 'NONE', #9746 ) ;
#16119 = CARTESIAN_POINT ( 'NONE',  ( 81.02178482187500208, -34.49062499938548854, -102.3871387122750889 ) ) ;
#16120 = SURFACE_STYLE_USAGE ( .BOTH. , #4196 ) ;
#16121 = CARTESIAN_POINT ( 'NONE',  ( 235.5999999999999375, -32.86874999877096570, 99.99999999999998579 ) ) ;
#16122 = CARTESIAN_POINT ( 'NONE',  ( 234.0999999999999375, -32.49374999877096570, -47.40192378864679768 ) ) ;
#16123 = EDGE_CURVE ( 'NONE', #10576, #12007, #8344, .T. ) ;
#16124 = CARTESIAN_POINT ( 'NONE',  ( -79.64356964374999848, -30.36562499938548498, 99.99999999999998579 ) ) ;
#16125 = ORIENTED_EDGE ( 'NONE', *, *, #6272, .T. ) ;
#16126 = VERTEX_POINT ( 'NONE', #10036 ) ;
#16127 = CARTESIAN_POINT ( 'NONE',  ( 105.1999999999999744, -4.999999999999976907, 153.0000000000000000 ) ) ;
#16128 = CARTESIAN_POINT ( 'NONE',  ( 244.7999999999999545, -32.00000000000000000, -100.0000000000000000 ) ) ;
#16129 = ORIENTED_EDGE ( 'NONE', *, *, #1257, .T. ) ;
#16130 = CARTESIAN_POINT ( 'NONE',  ( 0.6666666666666658525, -4.233901974057276085, -3.300726591567086476 ) ) ;
#16131 = CARTESIAN_POINT ( 'NONE',  ( 80.90000000000000568, -34.35000000000000853, -102.5980762113533018 ) ) ;
#16132 = CARTESIAN_POINT ( 'NONE',  ( 80.42036527867307427, -31.99999999999999289, -102.1983759483902645 ) ) ;
#16133 = CARTESIAN_POINT ( 'NONE',  ( -79.64356964375001269, -30.51562499938548711, 101.5914258081833879 ) ) ;
#16134 = CARTESIAN_POINT ( 'NONE',  ( -85.40000000000000568, -32.73750000000000426, 98.26794919243111792 ) ) ;
#16135 = CARTESIAN_POINT ( 'NONE',  ( 234.0999999999999375, -32.49374999877096570, -47.40192378864679768 ) ) ;
#16136 = AXIS2_PLACEMENT_3D ( 'NONE', #17487, #2722, #8484 ) ;
#16137 =( LENGTH_UNIT ( ) NAMED_UNIT ( * ) SI_UNIT ( .MILLI., .METRE. ) );
#16138 = CARTESIAN_POINT ( 'NONE',  ( -84.69814109749898989, -35.13162207320847585, 98.07164642868930571 ) ) ;
#16139 = CARTESIAN_POINT ( 'NONE',  ( -79.64356964374999848, -34.86562499938548143, 99.99999999999998579 ) ) ;
#16140 =( BOUNDED_CURVE ( )  B_SPLINE_CURVE ( 2, ( #502, #1857, #7815, #13963, #6455, #12408, #17579, #11610, #2334 ),
 .UNSPECIFIED., .F., .F. ) 
 B_SPLINE_CURVE_WITH_KNOTS ( ( 3, 2, 2, 2, 3 ),
 ( 0.02083333333333331136, 0.02777777777777777624, 0.04166666666666666435, 0.05555555555555555247, 0.06250000000000006939 ),
 .UNSPECIFIED. ) 
 CURVE ( )  GEOMETRIC_REPRESENTATION_ITEM ( )  RATIONAL_B_SPLINE_CURVE ( ( 0.9330127018922194093, 0.9330127018922191873, 1.000000000000000000, 0.8660254037844387076, 1.000000000000000000, 0.8660254037844387076, 1.000000000000000000, 0.9330127018922187432, 0.9330127018922194093 ) ) 
 REPRESENTATION_ITEM ( '' )  );
#16141 = CARTESIAN_POINT ( 'NONE',  ( -83.20384757729338787, -34.53615380933862866, -102.9999999999999858 ) ) ;
#16142 = ORIENTED_EDGE ( 'NONE', *, *, #5326, .T. ) ;
#16143 = CARTESIAN_POINT ( 'NONE',  ( -82.39999999999999147, -30.25312499938548783, -103.1828516163667899 ) ) ;
#16144 = CARTESIAN_POINT ( 'NONE',  ( -80.90000000000000568, -33.24374999877097281, 97.40192378864668399 ) ) ;
#16145 = CARTESIAN_POINT ( 'NONE',  ( 235.3564303562499447, -34.94062499938547717, 98.40857419181659793 ) ) ;
#16146 = CARTESIAN_POINT ( 'NONE',  ( -85.15643035624999868, -31.97812499938548925, 98.40857419181659793 ) ) ;
#16147 = FACE_OUTER_BOUND ( 'NONE', #9868, .T. ) ;
#16148 = CARTESIAN_POINT ( 'NONE',  ( 229.8435696437499871, -32.42812499938548143, -51.59142580818350865 ) ) ;
#16149 = AXIS2_PLACEMENT_3D ( 'NONE', #16375, #2799, #14905 ) ;
#16150 = ORIENTED_EDGE ( 'NONE', *, *, #10557, .T. ) ;
#16151 = ORIENTED_EDGE ( 'NONE', *, *, #6132, .T. ) ;
#16152 = FACE_BOUND ( 'NONE', #18107, .T. ) ;
#16153 = CARTESIAN_POINT ( 'NONE',  ( -81.02178482187500208, -32.99062499938548854, 97.61286128772489690 ) ) ;
#16154 = CARTESIAN_POINT ( 'NONE',  ( -82.65333140691201663, -34.99995246259153703, -102.9892844631211943 ) ) ;
#16155 = CARTESIAN_POINT ( 'NONE',  ( 81.02178482187500208, -34.79062499938548569, 102.3871387122750889 ) ) ;
#16156 = AXIS2_PLACEMENT_3D ( 'NONE', #6371, #5008, #16721 ) ;
#16157 = CARTESIAN_POINT ( 'NONE',  ( 83.90000000000000568, -33.97500000000000853, -102.5980762113533018 ) ) ;
#16158 = EDGE_CURVE ( 'NONE', #10474, #16790, #5647, .T. ) ;
#16159 = CARTESIAN_POINT ( 'NONE',  ( 231.2217848218749339, -32.01562499938548001, 97.61286128772489690 ) ) ;
#16160 = CARTESIAN_POINT ( 'NONE',  ( 229.8435696437499303, -33.74062499938548143, -50.00000000000011369 ) ) ;
#16161 = FACE_OUTER_BOUND ( 'NONE', #18643, .T. ) ;
#16162 = VECTOR ( 'NONE', #11598, 1000.000000000000000 ) ;
#16163 = CARTESIAN_POINT ( 'NONE',  ( 244.7999999999999545, -35.00000000000000000, 150.0000000000000000 ) ) ;
#16164 = AXIS2_PLACEMENT_3D ( 'NONE', #5547, #8456, #12766 ) ;
#16165 = CARTESIAN_POINT ( 'NONE',  ( 83.77821517812500929, -30.96562499938548640, -102.3871387122750889 ) ) ;
#16166 = CARTESIAN_POINT ( 'NONE',  ( 230.4884450829329694, -35.14114833091483803, -51.77179122389379984 ) ) ;
#16167 = CARTESIAN_POINT ( 'NONE',  ( -79.64356964374999848, -34.41562499938548569, 99.99999999999998579 ) ) ;
#16168 = CARTESIAN_POINT ( 'NONE',  ( 79.64356964375001269, -31.67812499938548143, -98.40857419181659793 ) ) ;
#16169 = ADVANCED_FACE ( 'NONE', ( #8463 ), #2411, .T. ) ;
#16170 = ORIENTED_EDGE ( 'NONE', *, *, #6640, .F. ) ;
#16171 = CYLINDRICAL_SURFACE ( 'NONE', #407, 2.199999999999993516 ) ;
#16172 = AXIS2_PLACEMENT_3D ( 'NONE', #1060, #18940, #14143 ) ;
#16173 = CARTESIAN_POINT ( 'NONE',  ( -82.65380294351676582, -34.99990492518305274, 97.01075526832239859 ) ) ;
#16174 = CARTESIAN_POINT ( 'NONE',  ( 231.2217848218749339, -31.52812499938548285, -47.61286128772501769 ) ) ;
#16175 = CARTESIAN_POINT ( 'NONE',  ( -81.02178482187500208, -32.24062499938548854, 102.3871387122750889 ) ) ;
#16176 = ORIENTED_EDGE ( 'NONE', *, *, #6023, .F. ) ;
#16177 = CARTESIAN_POINT ( 'NONE',  ( -79.39999999999999147, -32.88750000000000284, 98.26794919243110371 ) ) ;
#16178 = AXIS2_PLACEMENT_3D ( 'NONE', #12384, #18351, #15311 ) ;
#16179 = VECTOR ( 'NONE', #13142, 1000.000000000000000 ) ;
#16180 = CARTESIAN_POINT ( 'NONE',  ( 3.973110223765528914, 0.6902454861566582611, -3.565797985667391590 ) ) ;
#16181 = CARTESIAN_POINT ( 'NONE',  ( 69.99999999999998579, -34.99999999999999289, 150.0000000000000000 ) ) ;
#16182 = CARTESIAN_POINT ( 'NONE',  ( -79.39999999999999147, -33.40856250001229455, 101.7320508075688537 ) ) ;
#16183 = EDGE_CURVE ( 'NONE', #5568, #1884, #14227, .T. ) ;
#16184 = ADVANCED_FACE ( 'NONE', ( #11211, #14417 ), #2599, .F. ) ;
#16185 = CARTESIAN_POINT ( 'NONE',  ( 4.030867648404695025, 2.329326259788712772, -2.965488570641336974 ) ) ;
#16186 = CARTESIAN_POINT ( 'NONE',  ( -85.40000000000000568, -32.28750000000000142, 98.26794919243111792 ) ) ;
#16187 = CARTESIAN_POINT ( 'NONE',  ( -79.64356964375001269, -32.20312499938548001, 101.5914258081833879 ) ) ;
#16188 = DIRECTION ( 'NONE',  ( 1.000000000000000000, -4.625929269271485791E-17, 0.000000000000000000 ) ) ;
#16189 = CARTESIAN_POINT ( 'NONE',  ( 85.15643035624999868, -32.91562499938549280, 98.40857419181659793 ) ) ;
#16190 = EDGE_CURVE ( 'NONE', #5681, #5198, #12083, .T. ) ;
#16191 = FACE_OUTER_BOUND ( 'NONE', #16027, .T. ) ;
#16192 = CARTESIAN_POINT ( 'NONE',  ( 231.7961524227065695, -34.80134618820329706, 102.9999999999999858 ) ) ;
#16193 = CARTESIAN_POINT ( 'NONE',  ( 81.02178482187500208, -33.25312499938548427, -102.3871387122750889 ) ) ;
#16194 = VECTOR ( 'NONE', #3877, 1000.000000000000000 ) ;
#16195 = CARTESIAN_POINT ( 'NONE',  ( -79.64356964374999848, -31.37812499938548427, -99.99999999999998579 ) ) ;
#16196 = EDGE_LOOP ( 'NONE', ( #17031, #9784, #3273, #9549 ) ) ;
#16197 = CARTESIAN_POINT ( 'NONE',  ( 85.40000000000000568, -32.60624999877097707, 98.26794919243111792 ) ) ;
#16198 = LINE ( 'NONE', #273, #6170 ) ;
#16199 = CARTESIAN_POINT ( 'NONE',  ( 4.071447262713890680, -4.041451884327388555, 0.000000000000000000 ) ) ;
#16200 = FACE_OUTER_BOUND ( 'NONE', #13977, .T. ) ;
#16201 = CARTESIAN_POINT ( 'NONE',  ( 82.85293433259542439, -31.99999999999999289, 102.8010948079569005 ) ) ;
#16202 = EDGE_LOOP ( 'NONE', ( #16439, #4372, #18170 ) ) ;
#16203 = ADVANCED_FACE ( 'NONE', ( #8656 ), #19279, .T. ) ;
#16204 = CARTESIAN_POINT ( 'NONE',  ( -79.64356964374999848, -33.96562499938548285, -99.99999999999998579 ) ) ;
#16205 = CARTESIAN_POINT ( 'NONE',  ( 4.197310751797292738, 0.8178363989516252985, -3.502498386812444409 ) ) ;
#16206 = ORIENTED_EDGE ( 'NONE', *, *, #10017, .F. ) ;
#16207 = CARTESIAN_POINT ( 'NONE',  ( 79.64356964374999848, -34.98839802032724577, 99.56403331587401340 ) ) ;
#16208 = CARTESIAN_POINT ( 'NONE',  ( -85.15643035624999868, -34.34062499938548285, -101.5914258081833879 ) ) ;
#16209 = CARTESIAN_POINT ( 'NONE',  ( -80.24181665639368077, -31.99999999999999289, -102.0230471653775766 ) ) ;
#16210 = CARTESIAN_POINT ( 'NONE',  ( -80.90000000000000568, -32.04374999877096997, -97.40192378864668399 ) ) ;
#16211 = CARTESIAN_POINT ( 'NONE',  ( 233.9782151781249411, -31.00312499938548072, 102.3871387122750889 ) ) ;
#16212 = CARTESIAN_POINT ( 'NONE',  ( -82.39999999999999147, -35.00624999877097565, 96.53589838486223584 ) ) ;
#16213 = CARTESIAN_POINT ( 'NONE',  ( -81.02178482187500208, -34.00312499938548427, 97.61286128772489690 ) ) ;
#16214 = CARTESIAN_POINT ( 'NONE',  ( -81.02178482187500208, -34.34062499938548285, -102.3871387122750889 ) ) ;
#16215 = DIRECTION ( 'NONE',  ( -1.387778780781445676E-15, -1.000000000000000000, 0.000000000000000000 ) ) ;
#16216 = CARTESIAN_POINT ( 'NONE',  ( -82.39999999999999147, -34.33124999877097139, -97.00000000000000000 ) ) ;
#16217 = ADVANCED_FACE ( 'NONE', ( #4267 ), #13964, .F. ) ;
#16218 = CARTESIAN_POINT ( 'NONE',  ( 85.40000000000000568, -30.88124999877097210, -98.26794919243111792 ) ) ;
#16219 = CARTESIAN_POINT ( 'NONE',  ( 229.5999999999999375, -33.63749999999998863, 98.26794919243111792 ) ) ;
#16220 = ORIENTED_EDGE ( 'NONE', *, *, #47, .T. ) ;
#16221 = FACE_BOUND ( 'NONE', #1122, .T. ) ;
#16222 = SHAPE_REPRESENTATION_RELATIONSHIP ( 'NONE' , 'NONE' ,  #7631, #16944 ) ;
#16223 = CARTESIAN_POINT ( 'NONE',  ( 235.5999999999999943, -33.73124999877096286, 98.26794919243110371 ) ) ;
#16224 = CARTESIAN_POINT ( 'NONE',  ( 229.5999999999999375, -34.40624999877096002, -48.26794919243123161 ) ) ;
#16225 = CARTESIAN_POINT ( 'NONE',  ( -85.15643035625001289, -34.15312499938548285, 101.5914258081833879 ) ) ;
#16226 = ORIENTED_EDGE ( 'NONE', *, *, #6504, .F. ) ;
#16227 = ORIENTED_EDGE ( 'NONE', *, *, #14293, .F. ) ;
#16228 = CARTESIAN_POINT ( 'NONE',  ( -81.59615242270665192, -34.18259618943233136, -103.0000000000000000 ) ) ;
#16229 = CARTESIAN_POINT ( 'NONE',  ( -4.211405944401398038, -2.460460786169389902, -3.751298493805494072 ) ) ;
#16230 = CARTESIAN_POINT ( 'NONE',  ( 232.5999999999999375, -34.16249999999999432, -53.00000000000010658 ) ) ;
#16231 = VERTEX_POINT ( 'NONE', #9775 ) ;
#16232 = LINE ( 'NONE', #11917, #8580 ) ;
#16233 = CARTESIAN_POINT ( 'NONE',  ( 80.90000000000000568, -34.80000000000000426, -102.5980762113533018 ) ) ;
#16234 = CARTESIAN_POINT ( 'NONE',  ( 81.68701737470168212, -31.99999999999999289, -102.8119722220549619 ) ) ;
#16235 = CARTESIAN_POINT ( 'NONE',  ( -79.64356964374999848, -34.97812499938548569, 99.99999999999998579 ) ) ;
#16236 = CARTESIAN_POINT ( 'NONE',  ( -83.90000000000000568, -31.42500000000000071, 97.40192378864668399 ) ) ;
#16237 = CARTESIAN_POINT ( 'NONE',  ( -94.79999999999999716, 0.000000000000000000, 150.0000000000000000 ) ) ;
#16238 = CARTESIAN_POINT ( 'NONE',  ( 231.6947747743591037, -31.99999999999998579, -52.66702445726939885 ) ) ;
#16239 = CARTESIAN_POINT ( 'NONE',  ( 79.59365286754817248, -35.00000000000000711, 100.0710144471396319 ) ) ;
#16240 = CARTESIAN_POINT ( 'NONE',  ( 85.10336890117790176, -35.00000000000000000, 99.00607337841680078 ) ) ;
#16241 = CARTESIAN_POINT ( 'NONE',  ( -82.40000000000000568, -34.61250000000001137, -102.9999999999999858 ) ) ;
#16242 = VERTEX_POINT ( 'NONE', #5188 ) ;
#16243 =( LENGTH_UNIT ( ) NAMED_UNIT ( * ) SI_UNIT ( .MILLI., .METRE. ) );
#16244 = CARTESIAN_POINT ( 'NONE',  ( -81.02178482187500208, -30.29062499938548569, -102.3871387122750889 ) ) ;
#16245 = FACE_OUTER_BOUND ( 'NONE', #6603, .T. ) ;
#16246 = CARTESIAN_POINT ( 'NONE',  ( -79.64356964375001269, -30.85312499938548569, 101.5914258081833879 ) ) ;
#16247 = CARTESIAN_POINT ( 'NONE',  ( 80.90000000000000568, -32.40000000000000568, 102.5980762113533018 ) ) ;
#16248 = CARTESIAN_POINT ( 'NONE',  ( 231.2217848218749339, -33.36562499938548143, -52.38713871227520968 ) ) ;
#16249 = ORIENTED_EDGE ( 'NONE', *, *, #19189, .T. ) ;
#16250 = ORIENTED_EDGE ( 'NONE', *, *, #16523, .T. ) ;
#16251 = CARTESIAN_POINT ( 'NONE',  ( -79.39999999999999147, -34.76250000000000284, -98.26794919243113213 ) ) ;
#16252 = CARTESIAN_POINT ( 'NONE',  ( -79.39999999999999147, -31.57499999999999929, 99.99999999999998579 ) ) ;
#16253 = CARTESIAN_POINT ( 'NONE',  ( -82.39999999999999147, -30.95624999877097139, 96.53589838486223584 ) ) ;
#16254 = CARTESIAN_POINT ( 'NONE',  ( 84.51155491706698797, -35.14114833091483803, 101.7717912238936719 ) ) ;
#16255 = CARTESIAN_POINT ( 'NONE',  ( 105.2000000000000739, -34.99999999999999289, 147.7999999999999829 ) ) ;
#16256 = CARTESIAN_POINT ( 'NONE',  ( 235.3564303562499447, -31.22812499938548214, 98.40857419181659793 ) ) ;
#16257 =( BOUNDED_CURVE ( )  B_SPLINE_CURVE ( 2, ( #18469, #1952, #697, #18564, #11032, #16996, #3607, #9568, #7910 ),
 .UNSPECIFIED., .F., .F. ) 
 B_SPLINE_CURVE_WITH_KNOTS ( ( 3, 2, 2, 2, 3 ),
 ( 0.3958333333333334259, 0.4027777777777777901, 0.4166666666666666852, 0.4305555555555555802, 0.4375000000000000555 ),
 .UNSPECIFIED. ) 
 CURVE ( )  GEOMETRIC_REPRESENTATION_ITEM ( )  RATIONAL_B_SPLINE_CURVE ( ( 0.9330127018922192983, 0.9330127018922200755, 1.000000000000000000, 0.8660254037844387076, 1.000000000000000000, 0.8660254037844387076, 1.000000000000000000, 0.9330127018922187432, 0.9330127018922192983 ) ) 
 REPRESENTATION_ITEM ( '' )  );
#16258 = CARTESIAN_POINT ( 'NONE',  ( 229.8435696437499587, -33.70312499938548001, -48.40857419181671162 ) ) ;
#16259 = CARTESIAN_POINT ( 'NONE',  ( 79.64356964375001269, -34.37812499938548427, 101.5914258081833879 ) ) ;
#16260 = CARTESIAN_POINT ( 'NONE',  ( 79.64356964374999848, -31.71562499938548285, -99.99999999999998579 ) ) ;
#16261 = CARTESIAN_POINT ( 'NONE',  ( 229.8435696437499587, -35.11426541925032296, -51.00325264771200295 ) ) ;
#16262 = CARTESIAN_POINT ( 'NONE',  ( 82.39999999999999147, -33.62812499938549138, -103.1828516163667899 ) ) ;
#16263 = ORIENTED_EDGE ( 'NONE', *, *, #6848, .F. ) ;
#16264 = CARTESIAN_POINT ( 'NONE',  ( 110.9999999999999574, -21.80000000000003268, -139.9999999999999716 ) ) ;
#16265 = CARTESIAN_POINT ( 'NONE',  ( -83.20384757729337366, -34.80134618820331127, 103.0000000000000000 ) ) ;
#16266 = LINE ( 'NONE', #16558, #8218 ) ;
#16267 = CARTESIAN_POINT ( 'NONE',  ( -82.39999999999999147, -32.50312499938548427, 96.81714838363319586 ) ) ;
#16268 = EDGE_LOOP ( 'NONE', ( #17477, #6224, #7155, #13974 ) ) ;
#16269 = CARTESIAN_POINT ( 'NONE',  ( -4.154094228333820915, -2.398367420967594921, -3.721909803043257803 ) ) ;
#16270 = EDGE_CURVE ( 'NONE', #6543, #14497, #1171, .T. ) ;
#16271 = CARTESIAN_POINT ( 'NONE',  ( 232.5999999999999943, -32.72812499938547859, 103.1828516163667899 ) ) ;
#16272 = CARTESIAN_POINT ( 'NONE',  ( -82.40000000000000568, -30.73124999877097352, 103.0000000000000000 ) ) ;
#16273 = CARTESIAN_POINT ( 'NONE',  ( -85.40000000000000568, -31.79606250001229384, 99.99999999999998579 ) ) ;
#16274 = EDGE_CURVE ( 'NONE', #11529, #11625, #2053, .T. ) ;
#16275 = ADVANCED_FACE ( 'NONE', ( #12700 ), #14080, .F. ) ;
#16276 = CARTESIAN_POINT ( 'NONE',  ( 0.02993401039713966885, -3.373851915354620701, -1.156317065392240329 ) ) ;
#16277 = CARTESIAN_POINT ( 'NONE',  ( -83.20384757729337366, -32.15759618943233278, 103.0000000000000000 ) ) ;
#16278 = CARTESIAN_POINT ( 'NONE',  ( -83.77821517812500929, -32.31562499938548427, 102.3871387122750889 ) ) ;
#16279 = CARTESIAN_POINT ( 'NONE',  ( 234.0999999999999375, -32.09999999999999432, 102.5980762113533018 ) ) ;
#16280 = CARTESIAN_POINT ( 'NONE',  ( 82.39999999999999147, -32.39062499938548001, 96.81714838363319586 ) ) ;
#16281 = CYLINDRICAL_SURFACE ( 'NONE', #6487, 3.000000000000002665 ) ;
#16282 = CARTESIAN_POINT ( 'NONE',  ( 232.3466685930879123, -34.99995246259152282, 97.01071553687879145 ) ) ;
#16283 = LINE ( 'NONE', #4658, #16933 ) ;
#16284 = CARTESIAN_POINT ( 'NONE',  ( -85.15643035625001289, -31.60312499938548569, -99.99999999999998579 ) ) ;
#16285 = EDGE_LOOP ( 'NONE', ( #11536, #11859, #15671 ) ) ;
#16286 = CARTESIAN_POINT ( 'NONE',  ( 79.39999999999999147, -34.21874999877096712, 99.99999999999998579 ) ) ;
#16287 = CARTESIAN_POINT ( 'NONE',  ( -6.259644161404860030E-16, -4.618802153517027165, -5.000000000000000000 ) ) ;
#16288 = CYLINDRICAL_SURFACE ( 'NONE', #256, 3.000000000000002665 ) ;
#16289 = VECTOR ( 'NONE', #17690, 1000.000000000000000 ) ;
#16290 = EDGE_CURVE ( 'NONE', #18412, #10068, #14900, .T. ) ;
#16291 = CARTESIAN_POINT ( 'NONE',  ( -83.77821517812500929, -30.77812499938548640, 97.61286128772489690 ) ) ;
#16292 = CARTESIAN_POINT ( 'NONE',  ( -94.79999999999999716, -3.000000000000000000, 150.0000000000000000 ) ) ;
#16293 = VERTEX_POINT ( 'NONE', #1057 ) ;
#16294 = EDGE_CURVE ( 'NONE', #6637, #6661, #7012, .T. ) ;
#16295 = CARTESIAN_POINT ( 'NONE',  ( -85.15643035624999868, -33.32812499938548001, -101.5914258081833879 ) ) ;
#16296 = CARTESIAN_POINT ( 'NONE',  ( 81.59615242270663771, -32.51115380933863008, 96.99999999999998579 ) ) ;
#16297 = ORIENTED_EDGE ( 'NONE', *, *, #17417, .F. ) ;
#16298 = CARTESIAN_POINT ( 'NONE',  ( -79.39999999999999147, -30.22500000000000142, 99.99999999999998579 ) ) ;
#16299 = CARTESIAN_POINT ( 'NONE',  ( -79.64356964374999848, -32.27812499938548996, -99.99999999999998579 ) ) ;
#16300 = CARTESIAN_POINT ( 'NONE',  ( 232.5999999999999091, -34.38749999999999574, -47.00000000000011369 ) ) ;
#16301 = CARTESIAN_POINT ( 'NONE',  ( -85.40000000000000568, -32.15624999877096712, -98.26794919243111792 ) ) ;
#16302 = CARTESIAN_POINT ( 'NONE',  ( 229.8435696437499303, -32.95312499938548001, 99.99999999999998579 ) ) ;
#16303 = CARTESIAN_POINT ( 'NONE',  ( -82.39999999999999147, -32.53518749875867400, 103.4641016151377499 ) ) ;
#16304 = CARTESIAN_POINT ( 'NONE',  ( -85.15643035624999868, -34.71562499938548285, 101.5914258081833879 ) ) ;
#16305 = CARTESIAN_POINT ( 'NONE',  ( -79.64356964374998427, -34.82812499938548711, -101.5914258081833879 ) ) ;
#16306 = CARTESIAN_POINT ( 'NONE',  ( 99.99999999999995737, -21.80000000000003268, -137.3499999999999943 ) ) ;
#16307 = VECTOR ( 'NONE', #2476, 1000.000000000000000 ) ;
#16308 = AXIS2_PLACEMENT_3D ( 'NONE', #15713, #868, #3781 ) ;
#16309 = FACE_OUTER_BOUND ( 'NONE', #11675, .T. ) ;
#16310 = CARTESIAN_POINT ( 'NONE',  ( 79.39999999999999147, -32.83124999877097139, -98.26794919243110371 ) ) ;
#16311 = CARTESIAN_POINT ( 'NONE',  ( 232.5999999999999375, -33.26249999999999574, 96.53589838486223584 ) ) ;
#16312 = ORIENTED_EDGE ( 'NONE', *, *, #5541, .T. ) ;
#16313 = CARTESIAN_POINT ( 'NONE',  ( 234.0999999999999375, -34.74374999877096570, 102.5980762113533018 ) ) ;
#16314 = CARTESIAN_POINT ( 'NONE',  ( 231.2217848218749339, -30.32812499938548001, 97.61286128772489690 ) ) ;
#16315 = CARTESIAN_POINT ( 'NONE',  ( 229.5999999999999375, -33.50624999877096144, -48.26794919243123161 ) ) ;
#16316 = CARTESIAN_POINT ( 'NONE',  ( -79.64356964374998427, -33.47812499938547859, 98.40857419181659793 ) ) ;
#16317 = ORIENTED_EDGE ( 'NONE', *, *, #17717, .F. ) ;
#16318 = ORIENTED_EDGE ( 'NONE', *, *, #323, .T. ) ;
#16319 = CARTESIAN_POINT ( 'NONE',  ( -80.90000000000000568, -34.35000000000000853, -97.40192378864668399 ) ) ;
#16320 = VECTOR ( 'NONE', #7806, 1000.000000000000000 ) ;
#16321 = CARTESIAN_POINT ( 'NONE',  ( -4.000000000000000000, 0.8730739991738342143, -3.223134629628428893 ) ) ;
#16322 = CARTESIAN_POINT ( 'NONE',  ( 235.5999999999999943, -34.31249999999999289, -48.26794919243124582 ) ) ;
#16323 = VERTEX_POINT ( 'NONE', #18937 ) ;
#16324 = CARTESIAN_POINT ( 'NONE',  ( -79.90595866893275456, -34.99999999999999289, 101.1871036926522720 ) ) ;
#16325 = CARTESIAN_POINT ( 'NONE',  ( 231.7961524227065695, -33.90134618820329138, 103.0000000000000000 ) ) ;
#16326 = CARTESIAN_POINT ( 'NONE',  ( -85.15643035624999868, -33.36562499938548854, 101.5914258081833879 ) ) ;
#16327 = CARTESIAN_POINT ( 'NONE',  ( -82.39999999999999147, -31.68750000000000355, 103.4641016151377499 ) ) ;
#16328 = CARTESIAN_POINT ( 'NONE',  ( -79.39999999999999147, -32.00624999877096855, 101.7320508075688537 ) ) ;
#16329 = CARTESIAN_POINT ( 'NONE',  ( 99.99999999999997158, -29.80000000000000071, -100.0000000000000000 ) ) ;
#16330 = ADVANCED_FACE ( 'NONE', ( #13535 ), #19220, .T. ) ;
#16331 = CARTESIAN_POINT ( 'NONE',  ( -84.69814181805116959, -35.36146079493983052, 98.07164728741744852 ) ) ;
#16332 = CARTESIAN_POINT ( 'NONE',  ( -81.70916641599839636, -35.00000000000000000, -102.8868501612597726 ) ) ;
#16333 = CARTESIAN_POINT ( 'NONE',  ( 231.2217848218749339, -30.96562499938547930, 102.3871387122750889 ) ) ;
#16334 = ORIENTED_EDGE ( 'NONE', *, *, #16290, .T. ) ;
#16335 = CARTESIAN_POINT ( 'NONE',  ( -82.39999999999999147, -33.17812499938548854, -96.81714838363319586 ) ) ;
#16336 = CARTESIAN_POINT ( 'NONE',  ( 4.630153689607048761, 0.000000000000000000, 0.000000000000000000 ) ) ;
#16337 = CARTESIAN_POINT ( 'NONE',  ( 235.5999999999999375, -34.66874999877096286, -50.00000000000011369 ) ) ;
#16338 = CARTESIAN_POINT ( 'NONE',  ( 229.5999999999999375, -34.44374999877096144, 99.99999999999998579 ) ) ;
#16339 = CARTESIAN_POINT ( 'NONE',  ( -81.02178482187500208, -31.79062499938548925, 102.3871387122750889 ) ) ;
#16340 = CARTESIAN_POINT ( 'NONE',  ( -83.20384757729338787, -33.95759618943233704, 102.9999999999999858 ) ) ;
#16341 = CARTESIAN_POINT ( 'NONE',  ( 231.2217848218749339, -33.21562499938547575, -47.61286128772501769 ) ) ;
#16342 = ORIENTED_EDGE ( 'NONE', *, *, #7308, .F. ) ;
#16343 = ORIENTED_EDGE ( 'NONE', *, *, #15676, .F. ) ;
#16344 = CARTESIAN_POINT ( 'NONE',  ( 69.99999999999998579, -34.99999999999999289, 150.0000000000000000 ) ) ;
#16345 = CARTESIAN_POINT ( 'NONE',  ( -80.90000000000000568, -31.65000000000000568, 102.5980762113533018 ) ) ;
#16346 = CARTESIAN_POINT ( 'NONE',  ( -82.39999999999999147, -32.08124999877097139, 103.4641016151377499 ) ) ;
#16347 = CARTESIAN_POINT ( 'NONE',  ( 83.90000000000000568, -32.77499999999999858, 102.5980762113533018 ) ) ;
#16348 = CARTESIAN_POINT ( 'NONE',  ( -4.024497503033714452, 2.323544716729487813, -3.572167766733750582 ) ) ;
#16349 = CARTESIAN_POINT ( 'NONE',  ( 232.5999999999999375, -32.95312499938548001, 96.81714838363319586 ) ) ;
#16350 = CARTESIAN_POINT ( 'NONE',  ( 235.3564303562499447, -34.41562499938547859, -50.00000000000011369 ) ) ;
#16351 = CARTESIAN_POINT ( 'NONE',  ( 83.77821517812500929, -34.11562499938548854, 97.61286128772489690 ) ) ;
#16352 = CARTESIAN_POINT ( 'NONE',  ( 83.77821517812500929, -32.46562499938548285, -97.61286128772489690 ) ) ;
#16353 = EDGE_LOOP ( 'NONE', ( #6397, #18776 ) ) ;
#16354 = B_SPLINE_CURVE_WITH_KNOTS ( 'NONE', 3,
 ( #7493, #13448, #5744, #8762, #10238, #16201, #85, #2902, #8857, #15014, #14714, #7295, #19225, #5841, #11794, #14812, #1439, #13003 ),
 .UNSPECIFIED., .F., .F.,
 ( 4, 2, 2, 2, 2, 2, 2, 2, 4 ),
 ( 0.000000000000000000, 0.0007089252359835869531, 0.001417850471967173906, 0.002126775707950760968, 0.002835700943934347813, 0.003544626179917934657, 0.004253551415901521936, 0.004962476651885108780, 0.005671401887868695625 ),
 .UNSPECIFIED. ) ;
#16355 = CARTESIAN_POINT ( 'NONE',  ( 235.3564303562499447, -34.86562499938547433, -50.00000000000011369 ) ) ;
#16356 = CARTESIAN_POINT ( 'NONE',  ( -83.77821517812500929, -34.56562499938548427, 102.3871387122750889 ) ) ;
#16357 = CARTESIAN_POINT ( 'NONE',  ( 79.64356964375001269, -33.02812499938548285, -98.40857419181659793 ) ) ;
#16358 = ORIENTED_EDGE ( 'NONE', *, *, #9468, .T. ) ;
#16359 = DIRECTION ( 'NONE',  ( 0.000000000000000000, 0.000000000000000000, 1.000000000000000000 ) ) ;
#16360 = DIRECTION ( 'NONE',  ( 0.000000000000000000, 0.000000000000000000, 1.000000000000000000 ) ) ;
#16361 = CARTESIAN_POINT ( 'NONE',  ( 231.2217848218749339, -30.32812499938548001, -52.38713871227520968 ) ) ;
#16362 = CARTESIAN_POINT ( 'NONE',  ( -82.39999999999999147, -30.11250000000000426, 96.53589838486223584 ) ) ;
#16363 = ORIENTED_EDGE ( 'NONE', *, *, #15963, .F. ) ;
#16364 = FACE_OUTER_BOUND ( 'NONE', #4062, .T. ) ;
#16365 = EDGE_CURVE ( 'NONE', #6865, #5861, #6031, .T. ) ;
#16366 =( BOUNDED_CURVE ( )  B_SPLINE_CURVE ( 2, ( #10131, #18640, #7914, #13863, #11402, #6721, #12960, #15709, #2311 ),
 .UNSPECIFIED., .F., .F. ) 
 B_SPLINE_CURVE_WITH_KNOTS ( ( 3, 2, 2, 2, 3 ),
 ( 0.8125000000000000000, 0.8194444444444444198, 0.8333333333333333703, 0.8472222222222222099, 0.8530683953269213582 ),
 .UNSPECIFIED. ) 
 CURVE ( )  GEOMETRIC_REPRESENTATION_ITEM ( )  RATIONAL_B_SPLINE_CURVE ( ( 0.9330127018922194093, 0.9330127018922194093, 1.000000000000000000, 0.8660254037844387076, 1.000000000000000000, 0.8660254037844387076, 1.000000000000000000, 0.9436068149601996025, 0.9346881722405915305 ) ) 
 REPRESENTATION_ITEM ( '' )  );
#16367 = CARTESIAN_POINT ( 'NONE',  ( 232.5999999999999943, -34.75312499938547717, 96.81714838363319586 ) ) ;
#16368 = FACE_OUTER_BOUND ( 'NONE', #7139, .T. ) ;
#16369 = CARTESIAN_POINT ( 'NONE',  ( -83.90000000000000568, -31.27106250001229881, 102.5980762113533018 ) ) ;
#16370 = CARTESIAN_POINT ( 'NONE',  ( 110.0000000000000142, 20.19999999999997797, -140.0000000000000000 ) ) ;
#16371 = CARTESIAN_POINT ( 'NONE',  ( -80.90000000000000568, -32.49374999877097281, 102.5980762113533018 ) ) ;
#16372 = CARTESIAN_POINT ( 'NONE',  ( -82.39999999999999147, -30.92812499938548143, 103.1828516163667899 ) ) ;
#16373 = CARTESIAN_POINT ( 'NONE',  ( -79.39999999999999147, -32.96250000000000568, 101.7320508075688537 ) ) ;
#16374 = CARTESIAN_POINT ( 'NONE',  ( 85.15643035624999868, -32.46562499938548996, 98.40857419181659793 ) ) ;
#16375 = CARTESIAN_POINT ( 'NONE',  ( 111.5000000000000142, 12.69999999999998508, 50.00000000000001421 ) ) ;
#16376 = CARTESIAN_POINT ( 'NONE',  ( -81.02178482187500208, -32.35312499938548569, 102.3871387122750889 ) ) ;
#16377 = CARTESIAN_POINT ( 'NONE',  ( -79.64356964374999848, -32.27812499938548996, -99.99999999999998579 ) ) ;
#16378 = ORIENTED_EDGE ( 'NONE', *, *, #5320, .F. ) ;
#16379 = CARTESIAN_POINT ( 'NONE',  ( 79.64356964375001269, -31.34062499938548640, 101.5914258081833879 ) ) ;
#16380 = CARTESIAN_POINT ( 'NONE',  ( -2.000000000000006661, 3.464101615137750834, 0.000000000000000000 ) ) ;
#16381 = CARTESIAN_POINT ( 'NONE',  ( 231.2217848218749339, -34.37812499938547717, -52.38713871227520968 ) ) ;
#16382 = CIRCLE ( 'NONE', #18890, 2.649999999999980371 ) ;
#16383 = CARTESIAN_POINT ( 'NONE',  ( 4.142654963991903472, -2.035398498734322104, -3.525413613457253348 ) ) ;
#16384 = CARTESIAN_POINT ( 'NONE',  ( -79.64356964375001269, -31.41562499938548569, 101.5914258081833879 ) ) ;
#16385 = ORIENTED_EDGE ( 'NONE', *, *, #7576, .T. ) ;
#16386 = CARTESIAN_POINT ( 'NONE',  ( -83.90000000000000568, -31.42500000000000071, -102.5980762113533018 ) ) ;
#16387 = CARTESIAN_POINT ( 'NONE',  ( 3.950233766685291137, 0.7256672287179417591, -3.499999999999844125 ) ) ;
#16388 = CARTESIAN_POINT ( 'NONE',  ( -81.59615242270662350, -30.13259618943233775, 97.00000000000004263 ) ) ;
#16389 = CARTESIAN_POINT ( 'NONE',  ( -82.39999999999999147, -33.74062499938548854, -96.81714838363319586 ) ) ;
#16390 = B_SPLINE_CURVE_WITH_KNOTS ( 'NONE', 3,
 ( #8832, #18029, #153, #14789 ),
 .UNSPECIFIED., .F., .F.,
 ( 4, 4 ),
 ( 2.380739282167303683E-07, 0.002044882221487525839 ),
 .UNSPECIFIED. ) ;
#16391 = CARTESIAN_POINT ( 'NONE',  ( -84.11496519894568280, -32.00000000000000000, -102.1846009218959210 ) ) ;
#16392 = CARTESIAN_POINT ( 'NONE',  ( -80.90000000000000568, -30.69374999877097210, -97.40192378864668399 ) ) ;
#16393 = CARTESIAN_POINT ( 'NONE',  ( 231.2217848218749339, -31.97812499938548214, 102.3871387122750889 ) ) ;
#16394 = CARTESIAN_POINT ( 'NONE',  ( -85.40000000000000568, -30.88518749875867897, 98.26794919243111792 ) ) ;
#16395 = CARTESIAN_POINT ( 'NONE',  ( -83.77821517812500929, -33.32812499938548711, 102.3871387122750889 ) ) ;
#16396 = CARTESIAN_POINT ( 'NONE',  ( -79.39999999999999147, -31.61250000000000071, 101.7320508075688537 ) ) ;
#16397 = CARTESIAN_POINT ( 'NONE',  ( 83.77821517812500929, -32.76562499938548711, 97.61286128772489690 ) ) ;
#16398 = CARTESIAN_POINT ( 'NONE',  ( 110.0000000000000142, 10.19999999999997620, -140.0000000000000000 ) ) ;
#16399 = AXIS2_PLACEMENT_3D ( 'NONE', #10404, #14406, #6997 ) ;
#16400 = ADVANCED_FACE ( 'NONE', ( #7489 ), #7390, .F. ) ;
#16401 = FACE_OUTER_BOUND ( 'NONE', #1381, .T. ) ;
#16402 = CARTESIAN_POINT ( 'NONE',  ( 82.39999999999999147, -35.00624999877097565, -96.53589838486223584 ) ) ;
#16403 = CARTESIAN_POINT ( 'NONE',  ( 235.5999999999999943, -34.23749999999999716, 98.26794919243110371 ) ) ;
#16404 = ORIENTED_EDGE ( 'NONE', *, *, #12618, .T. ) ;
#16405 = CARTESIAN_POINT ( 'NONE',  ( 229.8435696437499587, -33.89062499938548001, -51.59142580818350154 ) ) ;
#16406 = CARTESIAN_POINT ( 'NONE',  ( 235.5999999999999943, -34.63124999877096144, 98.26794919243110371 ) ) ;
#16407 = CARTESIAN_POINT ( 'NONE',  ( 229.5999999999999375, -33.09374999877096002, -50.00000000000011369 ) ) ;
#16408 = ADVANCED_FACE ( 'NONE', ( #4558 ), #78, .F. ) ;
#16409 = CARTESIAN_POINT ( 'NONE',  ( -79.64356964374998427, -34.37812499938548427, 98.40857419181659793 ) ) ;
#16410 = ORIENTED_EDGE ( 'NONE', *, *, #14974, .F. ) ;
#16411 = ORIENTED_EDGE ( 'NONE', *, *, #3099, .F. ) ;
#16412 = CARTESIAN_POINT ( 'NONE',  ( 99.99999999999997158, -29.80000000000000071, -100.0000000000000000 ) ) ;
#16413 = AXIS2_PLACEMENT_3D ( 'NONE', #2839, #13191, #6957 ) ;
#16414 = CARTESIAN_POINT ( 'NONE',  ( -85.40000000000000568, -34.91250000000000142, 101.7320508075688821 ) ) ;
#16415 = LINE ( 'NONE', #10165, #16289 ) ;
#16416 = ORIENTED_EDGE ( 'NONE', *, *, #4504, .T. ) ;
#16417 = CARTESIAN_POINT ( 'NONE',  ( -83.90000000000000568, -31.81874999877096855, 97.40192378864668399 ) ) ;
#16418 = DIRECTION ( 'NONE',  ( -1.000000000000000000, 0.000000000000000000, 0.000000000000000000 ) ) ;
#16419 = CARTESIAN_POINT ( 'NONE',  ( -79.64356964375001269, -34.49062499938548854, 98.40857419181659793 ) ) ;
#16420 = CARTESIAN_POINT ( 'NONE',  ( -79.39999999999999147, -34.27499999999999858, 99.99999999999998579 ) ) ;
#16421 = CARTESIAN_POINT ( 'NONE',  ( -85.40000000000000568, -32.19374999877096855, 99.99999999999998579 ) ) ;
#16422 = DIRECTION ( 'NONE',  ( -0.000000000000000000, 0.000000000000000000, -1.000000000000000000 ) ) ;
#16423 = EDGE_CURVE ( 'NONE', #4279, #16577, #7674, .T. ) ;
#16424 =( LENGTH_UNIT ( ) NAMED_UNIT ( * ) SI_UNIT ( .MILLI., .METRE. ) );
#16425 = FACE_OUTER_BOUND ( 'NONE', #19098, .T. ) ;
#16426 = DIRECTION ( 'NONE',  ( 1.000000000000000000, 0.000000000000000000, 0.000000000000000000 ) ) ;
#16427 = EDGE_CURVE ( 'NONE', #15137, #8464, #16579, .T. ) ;
#16428 = AXIS2_PLACEMENT_3D ( 'NONE', #14751, #17596, #12909 ) ;
#16429 = CARTESIAN_POINT ( 'NONE',  ( 235.3564303562499447, -30.40312499938547575, 101.5914258081833879 ) ) ;
#16430 = EDGE_LOOP ( 'NONE', ( #19218, #86, #8858 ) ) ;
#16431 = CARTESIAN_POINT ( 'NONE',  ( -79.64356964375001269, -32.65312499938548285, -98.40857419181659793 ) ) ;
#16432 = CARTESIAN_POINT ( 'NONE',  ( -0.1756481739660520902, 4.720212674038980261, -3.469390959564065291 ) ) ;
#16433 = DIRECTION ( 'NONE',  ( 1.000000000000000000, 0.000000000000000000, 0.000000000000000000 ) ) ;
#16434 = CARTESIAN_POINT ( 'NONE',  ( 81.28488860390724824, -34.99999999999997868, -102.5271494742948164 ) ) ;
#16435 = CARTESIAN_POINT ( 'NONE',  ( -81.02178482187500208, -31.34062499938548996, 102.3871387122750889 ) ) ;
#16436 = CARTESIAN_POINT ( 'NONE',  ( 232.5999999999999375, -29.99999999999999645, 103.0000000000000000 ) ) ;
#16437 = CARTESIAN_POINT ( 'NONE',  ( 233.9782151781249411, -33.44062499938547717, -52.38713871227520968 ) ) ;
#16438 = ORIENTED_EDGE ( 'NONE', *, *, #14974, .T. ) ;
#16439 = ORIENTED_EDGE ( 'NONE', *, *, #217, .T. ) ;
#16440 = CARTESIAN_POINT ( 'NONE',  ( 0.1388410611046090037, -2.351840044243035610, 2.926493552096026018 ) ) ;
#16441 = ADVANCED_FACE ( 'NONE', ( #17761 ), #2899, .F. ) ;
#16442 = CARTESIAN_POINT ( 'NONE',  ( -83.90000000000000568, -31.27500000000000568, 102.5980762113533018 ) ) ;
#16443 = CARTESIAN_POINT ( 'NONE',  ( -83.90000000000000568, -33.01874999877097139, 102.5980762113533018 ) ) ;
#16444 = CARTESIAN_POINT ( 'NONE',  ( 79.39999999999999147, -31.98750000000000071, 101.7320508075688821 ) ) ;
#16445 = CARTESIAN_POINT ( 'NONE',  ( -79.93183330737464587, -32.00000000000002132, -98.31447495408076520 ) ) ;
#16446 = CARTESIAN_POINT ( 'NONE',  ( 231.2217848218749339, -33.36562499938548143, 97.61286128772489690 ) ) ;
#16447 = CARTESIAN_POINT ( 'NONE',  ( 231.2217848218749339, -34.71562499938547575, -52.38713871227520968 ) ) ;
#16448 = CIRCLE ( 'NONE', #6796, 2.500000000000000888 ) ;
#16449 = CARTESIAN_POINT ( 'NONE',  ( -82.40000000000000568, -32.08124999877097139, -97.00000000000000000 ) ) ;
#16450 = CARTESIAN_POINT ( 'NONE',  ( 85.15643035624999868, -30.62812499938548427, -98.40857419181659793 ) ) ;
#16451 = VERTEX_POINT ( 'NONE', #12174 ) ;
#16452 = CARTESIAN_POINT ( 'NONE',  ( 235.3564303562499447, -34.90312499938547575, -48.40857419181671162 ) ) ;
#16453 = EDGE_CURVE ( 'NONE', #592, #6950, #18716, .T. ) ;
#16454 = CARTESIAN_POINT ( 'NONE',  ( 80.90000000000000568, -34.29374999877096997, 97.40192378864668399 ) ) ;
#16455 = CARTESIAN_POINT ( 'NONE',  ( 83.77821517812500929, -33.21562499938548285, -102.3871387122750889 ) ) ;
#16456 = AXIS2_PLACEMENT_3D ( 'NONE', #1244, #12868, #11593 ) ;
#16457 = B_SPLINE_CURVE_WITH_KNOTS ( 'NONE', 3,
 ( #4890, #598, #10834, #1666, #13569, #3312, #3414, #3505 ),
 .UNSPECIFIED., .F., .F.,
 ( 4, 2, 2, 4 ),
 ( 0.005725059856848641743, 0.006314084072593626612, 0.006903108288338611481, 0.008081156719828581220 ),
 .UNSPECIFIED. ) ;
#16458 = CYLINDRICAL_SURFACE ( 'NONE', #9763, 3.000000000000002665 ) ;
#16459 = CARTESIAN_POINT ( 'NONE',  ( 235.5999999999999943, -32.90624999877096002, 101.7320508075688537 ) ) ;
#16460 = CARTESIAN_POINT ( 'NONE',  ( 231.2217848218749339, -30.77812499938548285, -52.38713871227520968 ) ) ;
#16461 = CARTESIAN_POINT ( 'NONE',  ( -80.90000000000000568, -31.50000000000000000, 97.40192378864668399 ) ) ;
#16462 = VERTEX_POINT ( 'NONE', #4662 ) ;
#16463 = CARTESIAN_POINT ( 'NONE',  ( -83.20384757729335945, -30.35759618943233917, 103.0000000000000000 ) ) ;
#16464 = CIRCLE ( 'NONE', #10529, 2.649999999999980371 ) ;
#16465 = CARTESIAN_POINT ( 'NONE',  ( 232.5999999999999375, -34.33124999877097139, 103.0000000000000000 ) ) ;
#16466 = CARTESIAN_POINT ( 'NONE',  ( 79.64356964374999848, -30.36562499938548498, 99.99999999999998579 ) ) ;
#16467 = CARTESIAN_POINT ( 'NONE',  ( -79.39999999999999147, -31.57106250001229242, 99.99999999999998579 ) ) ;
#16468 = VECTOR ( 'NONE', #19239, 1000.000000000000000 ) ;
#16469 = PRESENTATION_LAYER_ASSIGNMENT (  '', '', ( #2115 ) ) ;
#16470 = CARTESIAN_POINT ( 'NONE',  ( -4.197393957002303999, -7.773935952363655451E-14, -3.503767560748929810 ) ) ;
#16471 = DIRECTION ( 'NONE',  ( -1.000000000000000000, 0.000000000000000000, -0.000000000000000000 ) ) ;
#16472 = CARTESIAN_POINT ( 'NONE',  ( -81.02178482187500208, -32.54062499938548569, 97.61286128772489690 ) ) ;
#16473 = CARTESIAN_POINT ( 'NONE',  ( 229.7512376763114901, -35.00000000000000711, 100.5466586069346278 ) ) ;
#16474 = CARTESIAN_POINT ( 'NONE',  ( 85.15643035624999868, -33.36562499938548854, 98.40857419181659793 ) ) ;
#16475 = DIRECTION ( 'NONE',  ( 0.000000000000000000, -1.000000000000000000, 0.000000000000000000 ) ) ;
#16476 = AXIS2_PLACEMENT_3D ( 'NONE', #2808, #13538, #16099 ) ;
#16477 = DIRECTION ( 'NONE',  ( 0.000000000000000000, -0.000000000000000000, -1.000000000000000000 ) ) ;
#16478 = CARTESIAN_POINT ( 'NONE',  ( -85.15643035625001289, -32.05312499938548854, 99.99999999999998579 ) ) ;
#16479 = CARTESIAN_POINT ( 'NONE',  ( -79.64356964374999848, -30.47812499938548569, -99.99999999999998579 ) ) ;
#16480 = ORIENTED_EDGE ( 'NONE', *, *, #11264, .F. ) ;
#16481 = CARTESIAN_POINT ( 'NONE',  ( 85.40000000000000568, -34.89374999877097139, 99.99999999999998579 ) ) ;
#16482 = CARTESIAN_POINT ( 'NONE',  ( 244.7999999999999545, -5.000000000000000888, -103.0000000000000995 ) ) ;
#16483 = AXIS2_PLACEMENT_3D ( 'NONE', #1558, #4575, #4289 ) ;
#16484 =( BOUNDED_CURVE ( )  B_SPLINE_CURVE ( 2, ( #18303, #10672, #12433, #147, #15267, #4923, #3149, #241, #1603 ),
 .UNSPECIFIED., .F., .F. ) 
 B_SPLINE_CURVE_WITH_KNOTS ( ( 3, 2, 2, 2, 3 ),
 ( 0.6041666666666666297, 0.6111111111111111605, 0.6250000000000000000, 0.6388888888888888395, 0.6458333333333332593 ),
 .UNSPECIFIED. ) 
 CURVE ( )  GEOMETRIC_REPRESENTATION_ITEM ( )  RATIONAL_B_SPLINE_CURVE ( ( 0.9330127018922192983, 0.9330127018922187432, 1.000000000000000000, 0.8660254037844387076, 1.000000000000000000, 0.8660254037844387076, 1.000000000000000000, 0.9330127018922198534, 0.9330127018922192983 ) ) 
 REPRESENTATION_ITEM ( '' )  );
#16485 = VECTOR ( 'NONE', #1194, 1000.000000000000000 ) ;
#16486 = CARTESIAN_POINT ( 'NONE',  ( -83.77821517812500929, -32.12812499938548427, 97.61286128772489690 ) ) ;
#16487 = CARTESIAN_POINT ( 'NONE',  ( 80.90000000000000568, -33.69374999877096855, -97.40192378864668399 ) ) ;
#16488 = ORIENTED_EDGE ( 'NONE', *, *, #6489, .T. ) ;
#16489 = CARTESIAN_POINT ( 'NONE',  ( -79.39999999999999147, -31.08750000000000213, -101.7320508075688821 ) ) ;
#16490 = CARTESIAN_POINT ( 'NONE',  ( 244.7999999999999545, -32.00000000000000000, 150.0000000000000000 ) ) ;
#16491 = CARTESIAN_POINT ( 'NONE',  ( 79.39999999999999147, -33.73124999877096997, 101.7320508075688963 ) ) ;
#16492 = CARTESIAN_POINT ( 'NONE',  ( -81.02178482187500208, -33.70312499938548711, -97.61286128772489690 ) ) ;
#16493 = CARTESIAN_POINT ( 'NONE',  ( 244.7999999999999545, -32.00000000000000000, -100.0000000000000000 ) ) ;
#16494 = EDGE_CURVE ( 'NONE', #14497, #6753, #16198, .T. ) ;
#16495 = CARTESIAN_POINT ( 'NONE',  ( 233.9782151781249411, -30.85312499938547859, 97.61286128772489690 ) ) ;
#16496 = CARTESIAN_POINT ( 'NONE',  ( -79.39999999999999147, -31.56018749875868323, 101.7320508075688537 ) ) ;
#16497 = CARTESIAN_POINT ( 'NONE',  ( -79.64356964375001269, -34.04062499938549280, 98.40857419181659793 ) ) ;
#16498 = VECTOR ( 'NONE', #18095, 1000.000000000000000 ) ;
#16499 = CARTESIAN_POINT ( 'NONE',  ( 235.5999999999999943, -33.73124999877096286, 98.26794919243110371 ) ) ;
#16500 = CARTESIAN_POINT ( 'NONE',  ( 79.64356964374998427, -33.02812499938548285, 101.5914258081833879 ) ) ;
#16501 = PLANE ( 'NONE',  #4309 ) ;
#16502 = LINE ( 'NONE', #3105, #7396 ) ;
#16503 = CARTESIAN_POINT ( 'NONE',  ( 85.40000000000000568, -34.93124999877096570, -98.26794919243111792 ) ) ;
#16504 = CARTESIAN_POINT ( 'NONE',  ( 234.0999999999999375, -32.99999999999999289, 102.5980762113533018 ) ) ;
#16505 = ORIENTED_EDGE ( 'NONE', *, *, #8987, .T. ) ;
#16506 = CARTESIAN_POINT ( 'NONE',  ( 229.8435696437499587, -33.81562499938547717, -48.40857419181671162 ) ) ;
#16507 = CARTESIAN_POINT ( 'NONE',  ( 229.8435696437499303, -31.15312499938548285, 99.99999999999998579 ) ) ;
#16508 = CARTESIAN_POINT ( 'NONE',  ( 229.5999999999999375, -32.64374999877096428, -50.00000000000011369 ) ) ;
#16509 = CARTESIAN_POINT ( 'NONE',  ( -79.64356964374999848, -33.06562499938548427, 99.99999999999998579 ) ) ;
#16510 = ORIENTED_EDGE ( 'NONE', *, *, #14734, .T. ) ;
#16511 = EDGE_LOOP ( 'NONE', ( #2859, #11317, #14662, #11618 ) ) ;
#16512 = CARTESIAN_POINT ( 'NONE',  ( -79.58826230849687988, -32.00000000000094502, 98.95399275615287138 ) ) ;
#16513 = CARTESIAN_POINT ( 'NONE',  ( -4.000000000000000000, -2.512220745329312610, -3.469390707569719901 ) ) ;
#16514 = CARTESIAN_POINT ( 'NONE',  ( 5.599999999999999645, 4.041451884327382338, 0.000000000000000000 ) ) ;
#16515 = VERTEX_POINT ( 'NONE', #14809 ) ;
#16516 = CARTESIAN_POINT ( 'NONE',  ( -83.20384757729335945, -31.38615380933863008, 96.99999999999997158 ) ) ;
#16517 = DIRECTION ( 'NONE',  ( -0.000000000000000000, -1.000000000000000000, -0.000000000000000000 ) ) ;
#16518 = ADVANCED_FACE ( 'NONE', ( #5838 ), #4463, .F. ) ;
#16519 = CARTESIAN_POINT ( 'NONE',  ( -81.02178482187500208, -33.10312499938548569, 97.61286128772489690 ) ) ;
#16520 = CARTESIAN_POINT ( 'NONE',  ( -85.40000000000000568, -30.39374999877097139, 99.99999999999998579 ) ) ;
#16521 = CARTESIAN_POINT ( 'NONE',  ( -82.39999999999999147, -32.30624999877097281, 96.53589838486223584 ) ) ;
#16522 = CARTESIAN_POINT ( 'NONE',  ( -82.40000000000001990, -34.55624999877097281, 97.00000000000000000 ) ) ;
#16523 = EDGE_CURVE ( 'NONE', #11485, #8694, #10475, .T. ) ;
#16524 = CARTESIAN_POINT ( 'NONE',  ( -80.90000000000000568, -33.89999999999999858, 102.5980762113533018 ) ) ;
#16525 = CARTESIAN_POINT ( 'NONE',  ( 80.90000000000000568, -34.64999999999999858, -97.40192378864668399 ) ) ;
#16526 = DIRECTION ( 'NONE',  ( 0.000000000000000000, -1.000000000000000000, 0.000000000000000000 ) ) ;
#16527 = CARTESIAN_POINT ( 'NONE',  ( -79.73531137350346398, -35.00000000000000000, -101.0054374292560908 ) ) ;
#16528 = CARTESIAN_POINT ( 'NONE',  ( 231.2217848218749339, -31.56562499938547717, 97.61286128772489690 ) ) ;
#16529 = ORIENTED_EDGE ( 'NONE', *, *, #1284, .T. ) ;
#16530 = PRESENTATION_STYLE_ASSIGNMENT (( #18382 ) ) ;
#16531 = CARTESIAN_POINT ( 'NONE',  ( -79.64356964374999848, -33.96562499938548285, -99.99999999999998579 ) ) ;
#16532 = CARTESIAN_POINT ( 'NONE',  ( 234.0999999999999375, -32.39999999999999858, -52.59807621135342970 ) ) ;
#16533 = CARTESIAN_POINT ( 'NONE',  ( -84.69814161231455785, -35.39427329483935836, 98.07164704222795137 ) ) ;
#16534 =( BOUNDED_CURVE ( )  B_SPLINE_CURVE ( 2, ( #15836, #14260, #19057, #17398, #2448, #14167, #5586, #8403, #991, #11533, #12803, #12899, #17495 ),
 .UNSPECIFIED., .F., .F. ) 
 B_SPLINE_CURVE_WITH_KNOTS ( ( 3, 2, 2, 2, 2, 2, 3 ),
 ( 0.8530683953269213582, 0.8611111111111111605, 0.8750000000000000000, 0.8888888888888888395, 0.9027777777777777901, 0.9166666666666666297, 0.9258785004222062076 ),
 .UNSPECIFIED. ) 
 CURVE ( )  GEOMETRIC_REPRESENTATION_ITEM ( )  RATIONAL_B_SPLINE_CURVE ( ( 0.9346881722405915305, 0.9224185888242391052, 1.000000000000000000, 0.8660254037844387076, 1.000000000000000000, 0.8660254037844387076, 1.000000000000000000, 0.8660254037844387076, 1.000000000000000000, 0.8660254037844387076, 1.000000000000000000, 0.9111410770381633828, 0.9401538762233125901 ) ) 
 REPRESENTATION_ITEM ( '' )  );
#16535 = CARTESIAN_POINT ( 'NONE',  ( -84.70388354820684640, -35.00002705695768412, -101.9214814096701076 ) ) ;
#16536 = CARTESIAN_POINT ( 'NONE',  ( -81.02178482187500208, -33.44062499938548427, 97.61286128772489690 ) ) ;
#16537 = CARTESIAN_POINT ( 'NONE',  ( 85.40000000000000568, -33.18750000000000000, -98.26794919243111792 ) ) ;
#16538 = CARTESIAN_POINT ( 'NONE',  ( 235.3564303562499447, -34.86562499938547433, -50.00000000000011369 ) ) ;
#16540 = ADVANCED_FACE ( 'NONE', ( #6226 ), #2805, .T. ) ;
#16539 = VERTEX_POINT ( 'NONE', #8946 ) ;
#16541 = ORIENTED_EDGE ( 'NONE', *, *, #430, .T. ) ;
#16542 = LINE ( 'NONE', #1686, #5426 ) ;
#16543 = CARTESIAN_POINT ( 'NONE',  ( -80.90000000000000568, -31.05000000000000071, 97.40192378864668399 ) ) ;
#16544 = EDGE_CURVE ( 'NONE', #5897, #10972, #1348, .T. ) ;
#16545 = CARTESIAN_POINT ( 'NONE',  ( -79.39999999999999147, -31.93124999877096926, 98.26794919243110371 ) ) ;
#16546 = CARTESIAN_POINT ( 'NONE',  ( 82.39999999999999147, -31.23750000000000071, 96.53589838486223584 ) ) ;
#16547 = FACE_OUTER_BOUND ( 'NONE', #8311, .T. ) ;
#16548 = CARTESIAN_POINT ( 'NONE',  ( 232.5999999999999375, -34.97812499938547859, 103.1828516163667899 ) ) ;
#16549 = CARTESIAN_POINT ( 'NONE',  ( 233.9782151781249411, -34.94062499938547717, -47.61286128772501769 ) ) ;
#16550 = CARTESIAN_POINT ( 'NONE',  ( 80.60346964438562622, -31.99999999999999289, -97.67482724156225515 ) ) ;
#16551 = CARTESIAN_POINT ( 'NONE',  ( 82.39999999999999147, -32.27812499938548285, -103.1828516163667899 ) ) ;
#16552 = EDGE_LOOP ( 'NONE', ( #14263, #12775, #18896, #778 ) ) ;
#16553 = CARTESIAN_POINT ( 'NONE',  ( 234.0999999999999375, -32.54999999999999716, -47.40192378864679768 ) ) ;
#16554 = CARTESIAN_POINT ( 'NONE',  ( 85.40000000000000568, -34.95000000000000284, -99.99999999999998579 ) ) ;
#16555 = CARTESIAN_POINT ( 'NONE',  ( 79.64356964375001269, -32.20312499938548001, -101.5914258081833879 ) ) ;
#16556 = FACE_OUTER_BOUND ( 'NONE', #1920, .T. ) ;
#16557 = CARTESIAN_POINT ( 'NONE',  ( -81.59615242270662350, -34.57634618820329564, 96.99999999999997158 ) ) ;
#16558 = CARTESIAN_POINT ( 'NONE',  ( 99.99999999999994316, -35.00000000000000000, 150.0000000000000000 ) ) ;
#16559 = CARTESIAN_POINT ( 'NONE',  ( -79.39999999999999147, -30.71250000000000568, 101.7320508075688537 ) ) ;
#16560 = ORIENTED_EDGE ( 'NONE', *, *, #19190, .F. ) ;
#16561 = CARTESIAN_POINT ( 'NONE',  ( -85.34657078790640128, -35.00060087132568754, 100.6622129346251597 ) ) ;
#16562 = CARTESIAN_POINT ( 'NONE',  ( 232.9413037568957066, -34.96883842999723413, 102.9857998004476087 ) ) ;
#16563 = ADVANCED_FACE ( 'NONE', ( #6605 ), #3351, .F. ) ;
#16564 = CARTESIAN_POINT ( 'NONE',  ( 81.02178482187500208, -31.19062499938548427, 102.3871387122750889 ) ) ;
#16565 = CARTESIAN_POINT ( 'NONE',  ( -83.90000000000000568, -32.17106250001229739, 102.5980762113533018 ) ) ;
#16566 = ADVANCED_FACE ( 'NONE', ( #464 ), #16958, .F. ) ;
#16567 = B_SPLINE_CURVE_WITH_KNOTS ( 'NONE', 3,
 ( #11149, #17118, #8128, #5110, #9391, #10957 ),
 .UNSPECIFIED., .F., .F.,
 ( 4, 2, 4 ),
 ( 0.003358874760055550156, 0.004541967308452096383, 0.005725059856848641743 ),
 .UNSPECIFIED. ) ;
#16568 = DIRECTION ( 'NONE',  ( 0.000000000000000000, 0.000000000000000000, 1.000000000000000000 ) ) ;
#16569 = CARTESIAN_POINT ( 'NONE',  ( 235.2033360070649906, -32.00000000000000000, -48.51078102784442336 ) ) ;
#16570 = DIRECTION ( 'NONE',  ( 1.000000000000000000, 0.000000000000000000, 0.000000000000000000 ) ) ;
#16571 = CARTESIAN_POINT ( 'NONE',  ( 83.77821517812500929, -30.66562499938548569, 102.3871387122750889 ) ) ;
#16572 = CARTESIAN_POINT ( 'NONE',  ( 102.9999999999999858, -5.200000000000008171, 150.0000000000000000 ) ) ;
#16573 = EDGE_CURVE ( 'NONE', #10162, #12012, #15535, .T. ) ;
#16574 = CARTESIAN_POINT ( 'NONE',  ( 235.3564303562499447, -31.30312499938547788, -48.40857419181671162 ) ) ;
#16575 = CARTESIAN_POINT ( 'NONE',  ( -99.99999999999998579, -5.200000000000000178, -150.0000000000000000 ) ) ;
#16576 = CARTESIAN_POINT ( 'NONE',  ( -83.77821517812500929, -31.97812499938548925, -97.61286128772489690 ) ) ;
#16577 = VERTEX_POINT ( 'NONE', #3569 ) ;
#16578 = CARTESIAN_POINT ( 'NONE',  ( 83.77821517812500929, -30.62812499938548783, 97.61286128772489690 ) ) ;
#16579 = LINE ( 'NONE', #12076, #9592 ) ;
#16580 = CARTESIAN_POINT ( 'NONE',  ( -79.64356964374999848, -32.72812499938548569, 99.99999999999998579 ) ) ;
#16581 = DIRECTION ( 'NONE',  ( -1.000000000000000000, 1.387778780781445676E-15, 2.407412430484046130E-31 ) ) ;
#16582 = EDGE_LOOP ( 'NONE', ( #3332, #11748, #7920, #494, #2228, #3626, #12589, #271, #2340, #7589, #5370, #8639, #6790, #12172, #13892, #19197, #13695 ) ) ;
#16583 = CARTESIAN_POINT ( 'NONE',  ( -85.40000000000000568, -32.28750000000000142, -101.7320508075688679 ) ) ;
#16584 = CARTESIAN_POINT ( 'NONE',  ( 4.175813232069151226, -4.122719923832748101, -3.898053888241413974E-16 ) ) ;
#16585 = CARTESIAN_POINT ( 'NONE',  ( 85.40000000000000568, -34.89374999877097139, -99.99999999999998579 ) ) ;
#16586 = CARTESIAN_POINT ( 'NONE',  ( -85.15643035624999868, -33.44062499938548427, -101.5914258081833879 ) ) ;
#16587 = DIRECTION ( 'NONE',  ( 1.000000000000000000, 0.000000000000000000, 0.000000000000000000 ) ) ;
#16588 = CARTESIAN_POINT ( 'NONE',  ( 231.2217848218749339, -33.32812499938548001, 102.3871387122750889 ) ) ;
#16589 = CARTESIAN_POINT ( 'NONE',  ( -85.40000000000000568, -30.84768749875867755, 99.99999999999998579 ) ) ;
#16590 = CARTESIAN_POINT ( 'NONE',  ( -79.64356964374999848, -32.72812499938548569, 99.99999999999998579 ) ) ;
#16591 = CARTESIAN_POINT ( 'NONE',  ( 234.0999999999999375, -33.69374999877096144, 97.40192378864668399 ) ) ;
#16592 = CARTESIAN_POINT ( 'NONE',  ( 83.77821517812500929, -33.36562499938548854, 102.3871387122750889 ) ) ;
#16593 = CARTESIAN_POINT ( 'NONE',  ( 82.39999999999999147, -32.98124999877096286, 96.99999999999998579 ) ) ;
#16594 = CARTESIAN_POINT ( 'NONE',  ( 85.40000000000000568, -32.70000000000000284, -99.99999999999998579 ) ) ;
#16595 = CARTESIAN_POINT ( 'NONE',  ( 79.39999999999999147, -33.28124999877096712, -98.26794919243110371 ) ) ;
#16596 = CARTESIAN_POINT ( 'NONE',  ( 232.5999999999999375, -33.48749999999999716, 103.4641016151377499 ) ) ;
#16597 =( BOUNDED_CURVE ( )  B_SPLINE_CURVE ( 2, ( #8935, #16277, #4548, #14901, #8843, #16186, #12066, #3076, #1529 ),
 .UNSPECIFIED., .F., .F. ) 
 B_SPLINE_CURVE_WITH_KNOTS ( ( 3, 2, 2, 2, 3 ),
 ( 0.3958333333333334259, 0.4027777777777777901, 0.4166666666666666852, 0.4305555555555555802, 0.4375000000000000555 ),
 .UNSPECIFIED. ) 
 CURVE ( )  GEOMETRIC_REPRESENTATION_ITEM ( )  RATIONAL_B_SPLINE_CURVE ( ( 0.9330127018922192983, 0.9330127018922200755, 1.000000000000000000, 0.8660254037844387076, 1.000000000000000000, 0.8660254037844387076, 1.000000000000000000, 0.9330127018922187432, 0.9330127018922192983 ) ) 
 REPRESENTATION_ITEM ( '' )  );
#16598 = ORIENTED_EDGE ( 'NONE', *, *, #17204, .T. ) ;
#16599 = CARTESIAN_POINT ( 'NONE',  ( 229.8435696437499587, -33.36562499938548143, -48.40857419181671162 ) ) ;
#16600 = CARTESIAN_POINT ( 'NONE',  ( 0.000000000000000000, 0.000000000000000000, -199.9999999999999716 ) ) ;
#16601 = CARTESIAN_POINT ( 'NONE',  ( 232.5999999999999375, -30.81562499938547717, 96.81714838363319586 ) ) ;
#16602 = CARTESIAN_POINT ( 'NONE',  ( 232.5999999999999375, -34.78124999877096002, -46.53589838486234953 ) ) ;
#16603 = CARTESIAN_POINT ( 'NONE',  ( -81.02178482187500208, -33.89062499938548711, 97.61286128772489690 ) ) ;
#16604 = ORIENTED_EDGE ( 'NONE', *, *, #5307, .F. ) ;
#16605 = ORIENTED_EDGE ( 'NONE', *, *, #4396, .T. ) ;
#16606 = CARTESIAN_POINT ( 'NONE',  ( 4.170895651974600327, 2.054890354522691087, -3.559174498016439259 ) ) ;
#16607 = CARTESIAN_POINT ( 'NONE',  ( -4.203934362469166963, -1.640673743454851286, -3.598432614606932756 ) ) ;
#16608 = CARTESIAN_POINT ( 'NONE',  ( 4.142654963991906136, -4.070796997468642431, 2.739218076410093718E-16 ) ) ;
#16609 = ORIENTED_EDGE ( 'NONE', *, *, #1112, .T. ) ;
#16610 = CARTESIAN_POINT ( 'NONE',  ( -85.40000000000000568, -31.33124999877096784, 98.26794919243111792 ) ) ;
#16611 = PLANE ( 'NONE',  #16732 ) ;
#16612 = AXIS2_PLACEMENT_3D ( 'NONE', #3283, #18341, #7683 ) ;
#16613 = CARTESIAN_POINT ( 'NONE',  ( -85.15643035625001289, -34.75312499938548427, 99.99999999999998579 ) ) ;
#16614 = CARTESIAN_POINT ( 'NONE',  ( -79.39999999999999147, -33.33749999999999858, 98.26794919243110371 ) ) ;
#16615 = CARTESIAN_POINT ( 'NONE',  ( -85.40000000000000568, -32.68124999877097281, 98.26794919243111792 ) ) ;
#16616 = CARTESIAN_POINT ( 'NONE',  ( -82.40000000000001990, -33.88124999877096855, 103.0000000000000000 ) ) ;
#16617 = CARTESIAN_POINT ( 'NONE',  ( 4.000000000000000000, 0.000000000000000000, 0.000000000000000000 ) ) ;
#16618 = CARTESIAN_POINT ( 'NONE',  ( 234.0999999999999375, -33.44999999999999574, 102.5980762113533018 ) ) ;
#16619 = DIRECTION ( 'NONE',  ( 0.000000000000000000, -1.000000000000000000, 0.000000000000000000 ) ) ;
#16620 = CARTESIAN_POINT ( 'NONE',  ( -79.60045861139946055, -34.99999999999998579, -100.3117415790902101 ) ) ;
#16621 = CARTESIAN_POINT ( 'NONE',  ( 232.5999999999999375, -31.60312499938548214, 96.81714838363319586 ) ) ;
#16622 = ORIENTED_EDGE ( 'NONE', *, *, #14991, .F. ) ;
#16623 = CARTESIAN_POINT ( 'NONE',  ( -79.64356964375001269, -32.57812499938548001, -101.5914258081833879 ) ) ;
#16624 = CARTESIAN_POINT ( 'NONE',  ( 233.4038475772933339, -32.56740381056765443, -47.00000000000012079 ) ) ;
#16625 = VECTOR ( 'NONE', #15561, 1000.000000000000000 ) ;
#16626 = CIRCLE ( 'NONE', #6323, 2.100000000000000089 ) ;
#16627 = DIRECTION ( 'NONE',  ( 0.000000000000000000, 0.000000000000000000, 1.000000000000000000 ) ) ;
#16628 = CARTESIAN_POINT ( 'NONE',  ( 99.99999999999994316, -21.80000000000003268, -139.9999999999999716 ) ) ;
#16629 = DIRECTION ( 'NONE',  ( -0.000000000000000000, -1.000000000000000000, -0.000000000000000000 ) ) ;
#16630 = CARTESIAN_POINT ( 'NONE',  ( 235.3564303562499447, -34.45312499938548001, -48.40857419181671162 ) ) ;
#16631 = EDGE_CURVE ( 'NONE', #5198, #3185, #16080, .T. ) ;
#16632 = EDGE_CURVE ( 'NONE', #7899, #12012, #9329, .T. ) ;
#16633 = VERTEX_POINT ( 'NONE', #18524 ) ;
#16634 = ORIENTED_EDGE ( 'NONE', *, *, #10313, .T. ) ;
#16635 = CARTESIAN_POINT ( 'NONE',  ( -83.90000000000000568, -30.37500000000000355, 102.5980762113533018 ) ) ;
#16636 = CARTESIAN_POINT ( 'NONE',  ( -85.40000000000000568, -31.78124999877096712, 98.26794919243111792 ) ) ;
#16637 = CARTESIAN_POINT ( 'NONE',  ( 83.90000000000000568, -30.82500000000000284, 97.40192378864668399 ) ) ;
#16638 = CARTESIAN_POINT ( 'NONE',  ( 82.39999999999999147, -33.65624999877097423, 103.0000000000000000 ) ) ;
#16640 = CARTESIAN_POINT ( 'NONE',  ( 235.3564303562499447, -34.41562499938547859, 99.99999999999998579 ) ) ;
#16639 = VECTOR ( 'NONE', #17266, 1000.000000000000000 ) ;
#16641 = CARTESIAN_POINT ( 'NONE',  ( 85.15643035625001289, -32.09062499938548996, -98.40857419181659793 ) ) ;
#16642 = CARTESIAN_POINT ( 'NONE',  ( 82.14831453747926560, -31.99999999999997868, -97.14155664246067090 ) ) ;
#16643 = EDGE_CURVE ( 'NONE', #9852, #9264, #11086, .T. ) ;
#16644 = CARTESIAN_POINT ( 'NONE',  ( 82.39999999999999147, -34.30312499938548143, -96.81714838363319586 ) ) ;
#16645 = VERTEX_POINT ( 'NONE', #9632 ) ;
#16646 =( BOUNDED_CURVE ( )  B_SPLINE_CURVE ( 2, ( #5495, #11245, #3815, #8498, #11441, #6567, #12515, #18485, #11048 ),
 .UNSPECIFIED., .F., .F. ) 
 B_SPLINE_CURVE_WITH_KNOTS ( ( 3, 2, 2, 2, 3 ),
 ( 0.6041666666666667407, 0.6111111111111111605, 0.6250000000000000000, 0.6388888888888888395, 0.6458333333333331483 ),
 .UNSPECIFIED. ) 
 CURVE ( )  GEOMETRIC_REPRESENTATION_ITEM ( )  RATIONAL_B_SPLINE_CURVE ( ( 0.9330127018922192983, 0.9330127018922198534, 1.000000000000000000, 0.8660254037844387076, 1.000000000000000000, 0.8660254037844387076, 1.000000000000000000, 0.9330127018922209636, 0.9330127018922194093 ) ) 
 REPRESENTATION_ITEM ( '' )  );
#16647 = CARTESIAN_POINT ( 'NONE',  ( 231.0999999999999375, -33.52499999999999147, -47.40192378864679768 ) ) ;
#16648 = CARTESIAN_POINT ( 'NONE',  ( -83.20395887649198130, -35.00000000000002842, 102.6365808225363025 ) ) ;
#16649 = CARTESIAN_POINT ( 'NONE',  ( 79.64356964374999848, -32.61562499938548854, -99.99999999999998579 ) ) ;
#16650 = DIRECTION ( 'NONE',  ( 0.000000000000000000, 0.000000000000000000, -1.000000000000000000 ) ) ;
#16651 = CARTESIAN_POINT ( 'NONE',  ( -82.39999999999999147, -31.94062499938548427, 103.1828516163667899 ) ) ;
#16652 = CARTESIAN_POINT ( 'NONE',  ( 229.8435696437499871, -33.81562499938547717, -48.40857419181671162 ) ) ;
#16653 = CARTESIAN_POINT ( 'NONE',  ( -82.39999999999999147, -30.56250000000000355, 96.53589838486223584 ) ) ;
#16654 = EDGE_CURVE ( 'NONE', #2034, #15766, #10601, .T. ) ;
#16655 = EDGE_LOOP ( 'NONE', ( #3816, #2423, #514, #16385 ) ) ;
#16656 = CARTESIAN_POINT ( 'NONE',  ( -79.39542567806877571, -34.99994613746206085, 100.0094913129781560 ) ) ;
#16657 = CARTESIAN_POINT ( 'NONE',  ( 235.3564303562499447, -34.86562499938547433, 99.99999999999998579 ) ) ;
#16658 = CARTESIAN_POINT ( 'NONE',  ( -80.90000000000000568, -32.40000000000000568, 97.40192378864668399 ) ) ;
#16659 = CARTESIAN_POINT ( 'NONE',  ( -79.39999999999999147, -33.85856250001229029, 101.7320508075688537 ) ) ;
#16660 = CARTESIAN_POINT ( 'NONE',  ( -85.40000000000000568, -33.11250000000000426, -98.26794919243111792 ) ) ;
#16661 = CARTESIAN_POINT ( 'NONE',  ( -82.39999999999999147, -30.81562499938548427, 96.81714838363319586 ) ) ;
#16662 = CARTESIAN_POINT ( 'NONE',  ( -84.51155386534844638, -35.25364837475780888, 98.22820752270799005 ) ) ;
#16663 = CARTESIAN_POINT ( 'NONE',  ( 83.77821517812500929, -35.12812499938548427, 97.61286128772489690 ) ) ;
#16664 = CARTESIAN_POINT ( 'NONE',  ( 85.15643035624999868, -32.91562499938549280, -101.5914258081833879 ) ) ;
#16665 = CARTESIAN_POINT ( 'NONE',  ( 0.000000000000000000, 0.000000000000000000, 0.000000000000000000 ) ) ;
#16666 = CARTESIAN_POINT ( 'NONE',  ( -83.77821517812500929, -32.57812499938548711, 97.61286128772489690 ) ) ;
#16667 = CARTESIAN_POINT ( 'NONE',  ( -79.64356964375001269, -33.14062499938548711, -101.5914258081833879 ) ) ;
#16668 = EDGE_LOOP ( 'NONE', ( #11910, #5745, #2051, #6883 ) ) ;
#16669 = CARTESIAN_POINT ( 'NONE',  ( 82.39999999999999147, -35.00624999877097565, 103.4641016151377499 ) ) ;
#16670 = CARTESIAN_POINT ( 'NONE',  ( 4.033901012036491984, -2.321269032827139256, -2.979444097107483369 ) ) ;
#16671 = FACE_OUTER_BOUND ( 'NONE', #13634, .T. ) ;
#16672 = CARTESIAN_POINT ( 'NONE',  ( -79.64356964374999848, -30.92812499938548498, 99.99999999999998579 ) ) ;
#16673 =( BOUNDED_SURFACE ( )  B_SPLINE_SURFACE ( 1, 2, ( 
 ( #15135, #7709, #9266, #4793, #13668, #12202, #15233, #1848, #12783, #18555, #15624, #5371, #6544, #11021, #2231, #3887, #8287, #9559, #2036, #9853, #14238, #5170, #8100, #12587, #14053, #687, #9954, #876, #3697, #11117, #15815, #17085, #18752, #3598, #2424, #12876, #7996, #15525, #8196, #11220, #6639, #6839, #8384, #973, #18848, #13953, #14335, #12489, #9664, #17375, #18459, #2142, #5470, #14146, #17185, #11415, #12681, #5080, #780, #17284, #3988, #6736, #9756, #594, #15719, #16986, #18655, #5274, #2324, #6928, #3789, #11318, #8765, #8859, #15909, #1256, #13254, #2609, #9256, #12972, #4276, #11512, #4084, #14622, #17475, #16295, #10240, #18942, #7115, #10046, #14716, #17858, #5565, #11888, #19227, #7203, #8569, #13070, #2904, #10332, #2708, #5940, #16204, #16004, #4470, #2514, #14523, #8471, #14428, #1157, #1441, #19034, #4374, #11695, #5658, #11601, #7297, #14814, #5843, #11796, #17569, #5746, #13157, #4181, #10141, #16101, #17766, #1062, #19128, #2810, #7395, #7018, #17664, #8668, #1354, #13358, #13736 ),
 ( #13540, #8952, #13450, #4860, #15109, #7496, #18147, #1636, #16769, #14920, #7782, #12179, #12081, #6418, #375, #9145, #1913, #1547, #3385, #7876, #3091, #13827, #87, #280, #469, #10804, #10711, #6231, #10521, #16489, #18339, #12373, #6327, #12279, #9334, #4769, #10423, #15300, #16386, #3282, #2996, #7681, #16676, #6038, #11987, #17954, #9239, #4564, #13635, #9052, #1724, #15017, #10617, #18243, #7590, #182, #15202, #6131, #1820, #18058, #4668, #16583, #3187, #11290, #6710, #662, #17161, #17260, #4960, #9641, #2300, #10997, #8360, #2011, #12657, #564, #12463, #3674, #6521, #5350, #18629, #7970, #15499, #18434, #3767, #6907, #13927, #952, #8265, #15600, #16963, #2113, #3865, #18729, #11092, #14314, #5246, #5052, #12854, #10903, #3574, #16869, #3475, #9534, #9827, #8073, #12761, #755, #14027, #6611, #15696, #15791, #14214, #851, #12560, #14118, #2208, #18530, #5146, #17061, #6814, #9435, #8169, #11196, #2398, #15401, #9732, #16251, #4518, #13501, #3050, #18010, #7638, #5797, #14773, #2860, #17352 ) ),
 .UNSPECIFIED., .F., .F., .F. ) 
 B_SPLINE_SURFACE_WITH_KNOTS ( ( 2, 2 ),
 ( 3, 2, 2, 2, 2, 2, 2, 2, 2, 2, 2, 2, 2, 2, 2, 2, 2, 2, 2, 2, 2, 2, 2, 2, 2, 2, 2, 2, 2, 2, 2, 2, 2, 2, 2, 2, 2, 2, 2, 2, 2, 2, 2, 2, 2, 2, 2, 2, 2, 2, 2, 2, 2, 2, 2, 2, 2, 2, 2, 2, 2, 2, 2, 2, 2, 2, 2, 2, 3 ),
 ( 0.000000000000000000, 1.000000000000000000 ),
 ( 0.000000000000000000, 0.01388888888888888812, 0.02777777777777777624, 0.04166666666666666435, 0.05555555555555555247, 0.06944444444444444753, 0.08333333333333332871, 0.09722222222222222376, 0.1111111111111111049, 0.1250000000000000000, 0.1388888888888888951, 0.1527777777777777901, 0.1666666666666666574, 0.1805555555555555525, 0.1944444444444444475, 0.2083333333333333426, 0.2222222222222222099, 0.2361111111111111049, 0.2500000000000000000, 0.2638888888888888951, 0.2777777777777777901, 0.2916666666666666852, 0.3055555555555555802, 0.3194444444444444198, 0.3333333333333333148, 0.3472222222222222099, 0.3611111111111111049, 0.3750000000000000000, 0.3888888888888888951, 0.4027777777777777901, 0.4166666666666666852, 0.4305555555555555802, 0.4444444444444444198, 0.4583333333333333148, 0.4722222222222222099, 0.4861111111111111049, 0.5000000000000000000, 0.5138888888888888395, 0.5277777777777777901, 0.5416666666666666297, 0.5555555555555555802, 0.5694444444444444198, 0.5833333333333333703, 0.5972222222222222099, 0.6111111111111111605, 0.6250000000000000000, 0.6388888888888888395, 0.6527777777777777901, 0.6666666666666666297, 0.6805555555555555802, 0.6944444444444444198, 0.7083333333333333703, 0.7222222222222222099, 0.7361111111111111605, 0.7500000000000000000, 0.7638888888888888395, 0.7777777777777777901, 0.7916666666666666297, 0.8055555555555555802, 0.8194444444444444198, 0.8333333333333333703, 0.8472222222222222099, 0.8611111111111111605, 0.8750000000000000000, 0.8888888888888888395, 0.9027777777777777901, 0.9166666666666666297, 0.9258785066912882389, 0.9351372917582011501 ),
 .UNSPECIFIED. ) 
 GEOMETRIC_REPRESENTATION_ITEM ( )  RATIONAL_B_SPLINE_SURFACE ( (
 ( 1.000000000000000000, 0.8660254037844387076, 1.000000000000000000, 0.8660254037844387076, 1.000000000000000000, 0.8660254037844387076, 1.000000000000000000, 0.8660254037844387076, 1.000000000000000000, 0.8660254037844387076, 1.000000000000000000, 0.8660254037844387076, 1.000000000000000000, 0.8660254037844387076, 1.000000000000000000, 0.8660254037844387076, 1.000000000000000000, 0.8660254037844387076, 1.000000000000000000, 0.8660254037844387076, 1.000000000000000000, 0.8660254037844387076, 1.000000000000000000, 0.8660254037844387076, 1.000000000000000000, 0.8660254037844387076, 1.000000000000000000, 0.8660254037844387076, 1.000000000000000000, 0.8660254037844387076, 1.000000000000000000, 0.8660254037844387076, 1.000000000000000000, 0.8660254037844387076, 1.000000000000000000, 0.8660254037844387076, 1.000000000000000000, 0.8660254037844387076, 1.000000000000000000, 0.8660254037844387076, 1.000000000000000000, 0.8660254037844387076, 1.000000000000000000, 0.8660254037844387076, 1.000000000000000000, 0.8660254037844387076, 1.000000000000000000, 0.8660254037844387076, 1.000000000000000000, 0.8660254037844387076, 1.000000000000000000, 0.8660254037844387076, 1.000000000000000000, 0.8660254037844387076, 1.000000000000000000, 0.8660254037844387076, 1.000000000000000000, 0.8660254037844387076, 1.000000000000000000, 0.8660254037844387076, 1.000000000000000000, 0.8660254037844387076, 1.000000000000000000, 0.8660254037844387076, 1.000000000000000000, 0.8660254037844387076, 1.000000000000000000, 0.8660254037844387076, 1.000000000000000000, 0.8660254037844387076, 1.000000000000000000, 0.8660254037844387076, 1.000000000000000000, 0.8660254037844387076, 1.000000000000000000, 0.8660254037844387076, 1.000000000000000000, 0.8660254037844387076, 1.000000000000000000, 0.8660254037844387076, 1.000000000000000000, 0.8660254037844387076, 1.000000000000000000, 0.8660254037844387076, 1.000000000000000000, 0.8660254037844387076, 1.000000000000000000, 0.8660254037844387076, 1.000000000000000000, 0.8660254037844387076, 1.000000000000000000, 0.8660254037844387076, 1.000000000000000000, 0.8660254037844387076, 1.000000000000000000, 0.8660254037844387076, 1.000000000000000000, 0.8660254037844387076, 1.000000000000000000, 0.8660254037844387076, 1.000000000000000000, 0.8660254037844387076, 1.000000000000000000, 0.8660254037844387076, 1.000000000000000000, 0.8660254037844387076, 1.000000000000000000, 0.8660254037844387076, 1.000000000000000000, 0.8660254037844387076, 1.000000000000000000, 0.8660254037844387076, 1.000000000000000000, 0.8660254037844387076, 1.000000000000000000, 0.8660254037844387076, 1.000000000000000000, 0.8660254037844387076, 1.000000000000000000, 0.8660254037844387076, 1.000000000000000000, 0.8660254037844387076, 1.000000000000000000, 0.8660254037844387076, 1.000000000000000000, 0.8660254037844387076, 1.000000000000000000, 0.8660254037844387076, 1.000000000000000000, 0.8660254037844387076, 1.000000000000000000, 0.8660254037844387076, 1.000000000000000000, 0.9111410165655264848, 0.9401539157124900736, 0.9401539157124900736, 0.9401539157124900736),
 ( 1.000000000000000000, 0.8660254037844387076, 1.000000000000000000, 0.8660254037844387076, 1.000000000000000000, 0.8660254037844387076, 1.000000000000000000, 0.8660254037844387076, 1.000000000000000000, 0.8660254037844387076, 1.000000000000000000, 0.8660254037844387076, 1.000000000000000000, 0.8660254037844387076, 1.000000000000000000, 0.8660254037844387076, 1.000000000000000000, 0.8660254037844387076, 1.000000000000000000, 0.8660254037844387076, 1.000000000000000000, 0.8660254037844387076, 1.000000000000000000, 0.8660254037844387076, 1.000000000000000000, 0.8660254037844387076, 1.000000000000000000, 0.8660254037844387076, 1.000000000000000000, 0.8660254037844387076, 1.000000000000000000, 0.8660254037844387076, 1.000000000000000000, 0.8660254037844387076, 1.000000000000000000, 0.8660254037844387076, 1.000000000000000000, 0.8660254037844387076, 1.000000000000000000, 0.8660254037844387076, 1.000000000000000000, 0.8660254037844387076, 1.000000000000000000, 0.8660254037844387076, 1.000000000000000000, 0.8660254037844387076, 1.000000000000000000, 0.8660254037844387076, 1.000000000000000000, 0.8660254037844387076, 1.000000000000000000, 0.8660254037844387076, 1.000000000000000000, 0.8660254037844387076, 1.000000000000000000, 0.8660254037844387076, 1.000000000000000000, 0.8660254037844387076, 1.000000000000000000, 0.8660254037844387076, 1.000000000000000000, 0.8660254037844387076, 1.000000000000000000, 0.8660254037844387076, 1.000000000000000000, 0.8660254037844387076, 1.000000000000000000, 0.8660254037844387076, 1.000000000000000000, 0.8660254037844387076, 1.000000000000000000, 0.8660254037844387076, 1.000000000000000000, 0.8660254037844387076, 1.000000000000000000, 0.8660254037844387076, 1.000000000000000000, 0.8660254037844387076, 1.000000000000000000, 0.8660254037844387076, 1.000000000000000000, 0.8660254037844387076, 1.000000000000000000, 0.8660254037844387076, 1.000000000000000000, 0.8660254037844387076, 1.000000000000000000, 0.8660254037844387076, 1.000000000000000000, 0.8660254037844387076, 1.000000000000000000, 0.8660254037844387076, 1.000000000000000000, 0.8660254037844387076, 1.000000000000000000, 0.8660254037844387076, 1.000000000000000000, 0.8660254037844387076, 1.000000000000000000, 0.8660254037844387076, 1.000000000000000000, 0.8660254037844387076, 1.000000000000000000, 0.8660254037844387076, 1.000000000000000000, 0.8660254037844387076, 1.000000000000000000, 0.8660254037844387076, 1.000000000000000000, 0.8660254037844387076, 1.000000000000000000, 0.8660254037844387076, 1.000000000000000000, 0.8660254037844387076, 1.000000000000000000, 0.8660254037844387076, 1.000000000000000000, 0.8660254037844387076, 1.000000000000000000, 0.8660254037844387076, 1.000000000000000000, 0.8660254037844387076, 1.000000000000000000, 0.8660254037844387076, 1.000000000000000000, 0.8660254037844387076, 1.000000000000000000, 0.8660254037844387076, 1.000000000000000000, 0.8660254037844387076, 1.000000000000000000, 0.8660254037844387076, 1.000000000000000000, 0.9111410165655264848, 0.9401539157124900736, 0.9401539157124900736, 0.9401539157124900736) ) ) 
 REPRESENTATION_ITEM ( '' )  SURFACE ( )  );
#16674 = CARTESIAN_POINT ( 'NONE',  ( 82.39999999999999147, -33.20624999877097849, 102.9999999999999858 ) ) ;
#16675 = ORIENTED_EDGE ( 'NONE', *, *, #10187, .F. ) ;
#16676 = CARTESIAN_POINT ( 'NONE',  ( -79.39999999999999147, -31.57499999999999929, -99.99999999999998579 ) ) ;
#16677 = CARTESIAN_POINT ( 'NONE',  ( 110.0000000000000000, 10.19999999999997620, -142.6499999999999773 ) ) ;
#16678 = CARTESIAN_POINT ( 'NONE',  ( 5.599999999999999645, 2.020725942163688504, 3.500000000000000000 ) ) ;
#16679 = EDGE_CURVE ( 'NONE', #10996, #7898, #18092, .T. ) ;
#16680 = CARTESIAN_POINT ( 'NONE',  ( 244.7999999999999545, -29.80000000000002203, 147.7999999999999829 ) ) ;
#16681 = CARTESIAN_POINT ( 'NONE',  ( 233.9782151781249411, -34.45312499938548001, 97.61286128772489690 ) ) ;
#16682 = CARTESIAN_POINT ( 'NONE',  ( -85.40000000000000568, -32.23518749875868394, 98.26794919243111792 ) ) ;
#16683 = ORIENTED_EDGE ( 'NONE', *, *, #4465, .T. ) ;
#16684 = LINE ( 'NONE', #4869, #12423 ) ;
#16685 = CARTESIAN_POINT ( 'NONE',  ( 79.39999999999999147, -32.86874999877097281, -99.99999999999998579 ) ) ;
#16686 = CARTESIAN_POINT ( 'NONE',  ( 79.64356964374998427, -34.45312499938548711, 98.40857419181659793 ) ) ;
#16687 = CARTESIAN_POINT ( 'NONE',  ( 234.0999999999999375, -33.39374999877096428, 102.5980762113533018 ) ) ;
#16688 = CARTESIAN_POINT ( 'NONE',  ( 82.39999999999999147, -33.20624999877097139, -96.53589838486223584 ) ) ;
#16689 = LINE ( 'NONE', #13841, #12716 ) ;
#16690 = VERTEX_POINT ( 'NONE', #5532 ) ;
#16691 = CARTESIAN_POINT ( 'NONE',  ( 229.8435696437499587, -34.34062499938547575, -51.59142580818350154 ) ) ;
#16692 =( NAMED_UNIT ( * ) SI_UNIT ( $, .STERADIAN. ) SOLID_ANGLE_UNIT ( ) );
#16693 = CARTESIAN_POINT ( 'NONE',  ( 229.5999999999999375, -34.44374999877096144, 99.99999999999998579 ) ) ;
#16694 = CARTESIAN_POINT ( 'NONE',  ( 233.9782151781249411, -30.85312499938547859, -52.38713871227520968 ) ) ;
#16695 = CARTESIAN_POINT ( 'NONE',  ( 235.5999999999999943, -34.68749999999999289, -51.73205080756900287 ) ) ;
#16696 = ORIENTED_EDGE ( 'NONE', *, *, #7308, .T. ) ;
#16697 = ORIENTED_EDGE ( 'NONE', *, *, #16632, .T. ) ;
#16698 = CARTESIAN_POINT ( 'NONE',  ( 4.000000000000000000, 2.309401076758497151, -3.433295621305379353 ) ) ;
#16699 = CARTESIAN_POINT ( 'NONE',  ( 4.071447262713887127, 2.020725942163686728, -3.499999999999999556 ) ) ;
#16700 = DIRECTION ( 'NONE',  ( 0.000000000000000000, 0.5000000000000007772, -0.8660254037844381525 ) ) ;
#16701 = ORIENTED_EDGE ( 'NONE', *, *, #13311, .F. ) ;
#16702 = ADVANCED_BREP_SHAPE_REPRESENTATION ( '', ( #9400, #10540 ), #4929 ) ;
#16703 = DIRECTION ( 'NONE',  ( 0.000000000000000000, -1.000000000000000000, 0.000000000000000000 ) ) ;
#16704 = FACE_OUTER_BOUND ( 'NONE', #1322, .T. ) ;
#16705 = CIRCLE ( 'NONE', #2025, 5.199999999999996625 ) ;
#16706 = CARTESIAN_POINT ( 'NONE',  ( -79.39999999999999147, -32.02500000000000568, 99.99999999999998579 ) ) ;
#16707 = CARTESIAN_POINT ( 'NONE',  ( -85.40000000000000568, -30.88124999877097210, 98.26794919243111792 ) ) ;
#16708 = CARTESIAN_POINT ( 'NONE',  ( -79.39999999999999147, -30.58124999877096784, 98.26794919243110371 ) ) ;
#16709 = DIRECTION ( 'NONE',  ( -0.5000000000000016653, 0.8660254037844378194, 0.000000000000000000 ) ) ;
#16710 =( BOUNDED_CURVE ( )  B_SPLINE_CURVE ( 2, ( #13199, #1582, #10086, #13487, #17997, #1483, #17702, #16141, #4507 ),
 .UNSPECIFIED., .F., .F. ) 
 B_SPLINE_CURVE_WITH_KNOTS ( ( 3, 2, 2, 2, 3 ),
 ( 0.7291666666666666297, 0.7361111111111111605, 0.7500000000000000000, 0.7638888888888888395, 0.7708333333333331483 ),
 .UNSPECIFIED. ) 
 CURVE ( )  GEOMETRIC_REPRESENTATION_ITEM ( )  RATIONAL_B_SPLINE_CURVE ( ( 0.9330127018922192983, 0.9330127018922187432, 1.000000000000000000, 0.8660254037844387076, 1.000000000000000000, 0.8660254037844387076, 1.000000000000000000, 0.9330127018922209636, 0.9330127018922194093 ) ) 
 REPRESENTATION_ITEM ( '' )  );
#16711 = DIRECTION ( 'NONE',  ( 0.000000000000000000, 0.000000000000000000, -1.000000000000000000 ) ) ;
#16712 = CARTESIAN_POINT ( 'NONE',  ( 3.878096787214571517, 3.381939201670113082, 1.142309474598439234 ) ) ;
#16713 = CARTESIAN_POINT ( 'NONE',  ( 4.000000000000000000, -2.309401076758516691, -0.4999999999999995559 ) ) ;
#16714 = CARTESIAN_POINT ( 'NONE',  ( 235.3564303562499447, -32.61562499938548143, 99.99999999999998579 ) ) ;
#16715 = ORIENTED_EDGE ( 'NONE', *, *, #16631, .F. ) ;
#16716 = CARTESIAN_POINT ( 'NONE',  ( -83.77821517812500929, -33.66562499938548569, -97.61286128772489690 ) ) ;
#16717 = CARTESIAN_POINT ( 'NONE',  ( -81.59615242270665192, -32.77634618820330559, -103.0000000000000000 ) ) ;
#16718 = ORIENTED_EDGE ( 'NONE', *, *, #3518, .F. ) ;
#16719 = VECTOR ( 'NONE', #15679, 1000.000000000000000 ) ;
#16720 = CARTESIAN_POINT ( 'NONE',  ( -82.40000000000000568, -33.43124999877096570, 102.9999999999999858 ) ) ;
#16721 = DIRECTION ( 'NONE',  ( 0.000000000000000000, 0.000000000000000000, 1.000000000000000000 ) ) ;
#16722 = CARTESIAN_POINT ( 'NONE',  ( 4.000000000000000000, 0.3987449864460005378, -0.01220643443059817035 ) ) ;
#16723 = ORIENTED_EDGE ( 'NONE', *, *, #7315, .T. ) ;
#16724 = ORIENTED_EDGE ( 'NONE', *, *, #13630, .T. ) ;
#16725 = DIRECTION ( 'NONE',  ( -0.000000000000000000, -1.000000000000000000, -0.000000000000000000 ) ) ;
#16726 = CARTESIAN_POINT ( 'NONE',  ( 79.39999999999999147, -31.16250000000000497, -101.7320508075688537 ) ) ;
#16727 = AXIS2_PLACEMENT_3D ( 'NONE', #1564, #10634, #15128 ) ;
#16728 = CARTESIAN_POINT ( 'NONE',  ( -83.90000000000000568, -35.26874999877097139, 102.5980762113533018 ) ) ;
#16729 = CARTESIAN_POINT ( 'NONE',  ( 79.39999999999999147, -32.43750000000000000, 101.7320508075688821 ) ) ;
#16730 = DIRECTION ( 'NONE',  ( 1.000000000000000000, 0.000000000000000000, -9.251858538542962756E-15 ) ) ;
#16731 = CARTESIAN_POINT ( 'NONE',  ( 231.2217848218749339, -35.01562499938548001, 102.3871387122750889 ) ) ;
#16732 = AXIS2_PLACEMENT_3D ( 'NONE', #3218, #2934, #7523 ) ;
#16733 = CARTESIAN_POINT ( 'NONE',  ( 84.44763168836730927, -32.00000000000000711, -101.8452947671444093 ) ) ;
#16734 = DIRECTION ( 'NONE',  ( -1.000000000000000000, 1.387778780781445478E-15, 2.407412430484046130E-31 ) ) ;
#16735 = B_SPLINE_CURVE_WITH_KNOTS ( 'NONE', 3,
 ( #8459, #5458, #7004, #8370, #6916 ),
 .UNSPECIFIED., .F., .F.,
 ( 4, 1, 4 ),
 ( 0.000000000000000000, 0.002309401076758505790, 0.004618802153517011580 ),
 .UNSPECIFIED. ) ;
#16736 = CARTESIAN_POINT ( 'NONE',  ( 85.15643035625001289, -32.84062499938548285, -99.99999999999998579 ) ) ;
#16737 = ORIENTED_EDGE ( 'NONE', *, *, #1608, .T. ) ;
#16738 = CARTESIAN_POINT ( 'NONE',  ( 232.5999999999999375, -33.48749999999999716, -46.53589838486234953 ) ) ;
#16739 = CARTESIAN_POINT ( 'NONE',  ( -80.90000000000000568, -33.75000000000000000, 97.40192378864668399 ) ) ;
#16740 = CARTESIAN_POINT ( 'NONE',  ( -83.90000000000000568, -30.82500000000000284, 102.5980762113533018 ) ) ;
#16741 = DIRECTION ( 'NONE',  ( -1.000000000000000000, 0.000000000000000000, 0.000000000000000000 ) ) ;
#16742 = CARTESIAN_POINT ( 'NONE',  ( -81.02178482187500208, -30.40312499938548640, 97.61286128772489690 ) ) ;
#16743 = CARTESIAN_POINT ( 'NONE',  ( 232.5999999999999375, -33.51562499938548001, -53.18285161636690361 ) ) ;
#16744 = CARTESIAN_POINT ( 'NONE',  ( -82.39999999999999147, -31.01249999999999929, 96.53589838486223584 ) ) ;
#16745 = EDGE_LOOP ( 'NONE', ( #13834, #9981 ) ) ;
#16746 = CYLINDRICAL_SURFACE ( 'NONE', #11030, 2.649999999999985700 ) ;
#16747 = CARTESIAN_POINT ( 'NONE',  ( -84.69814161231455785, -35.39427329483935836, 98.07164704222793716 ) ) ;
#16748 = CARTESIAN_POINT ( 'NONE',  ( 82.39999999999999147, -31.15312499938548640, 103.1828516163667899 ) ) ;
#16749 = CARTESIAN_POINT ( 'NONE',  ( 85.16931825408417467, -32.00000000000002132, -100.2387112178441555 ) ) ;
#16750 = CARTESIAN_POINT ( 'NONE',  ( -82.39999999999999147, -32.39062499938548711, 103.1828516163667899 ) ) ;
#16751 = AXIS2_PLACEMENT_3D ( 'NONE', #8208, #2240, #5182 ) ;
#16752 = CARTESIAN_POINT ( 'NONE',  ( 230.1446115142671260, -35.00000000000138556, 98.27756861396923682 ) ) ;
#16753 = CARTESIAN_POINT ( 'NONE',  ( 82.39999999999999147, -30.92812499938548143, 96.81714838363319586 ) ) ;
#16754 = ADVANCED_FACE ( 'NONE', ( #11284 ), #7, .F. ) ;
#16755 = CARTESIAN_POINT ( 'NONE',  ( 79.64356964375001269, -30.89062499938548711, -98.40857419181659793 ) ) ;
#16756 = CARTESIAN_POINT ( 'NONE',  ( 233.9782151781249411, -31.34062499938548285, -47.61286128772501769 ) ) ;
#16757 = CARTESIAN_POINT ( 'NONE',  ( -85.15643035625001289, -34.26562499938548711, 101.5914258081833879 ) ) ;
#16758 = CARTESIAN_POINT ( 'NONE',  ( -81.02178482187500208, -32.65312499938548996, -102.3871387122750889 ) ) ;
#16759 =( BOUNDED_CURVE ( )  B_SPLINE_CURVE ( 2, ( #2091, #6498, #8245, #3653, #5129, #542, #834, #5034, #643 ),
 .UNSPECIFIED., .F., .F. ) 
 B_SPLINE_CURVE_WITH_KNOTS ( ( 3, 2, 2, 2, 3 ),
 ( 0.6875000000000000000, 0.6944444444444444198, 0.7083333333333333703, 0.7222222222222222099, 0.7291666666666667407 ),
 .UNSPECIFIED. ) 
 CURVE ( )  GEOMETRIC_REPRESENTATION_ITEM ( )  RATIONAL_B_SPLINE_CURVE ( ( 0.9330127018922194093, 0.9330127018922194093, 1.000000000000000000, 0.8660254037844387076, 1.000000000000000000, 0.8660254037844387076, 1.000000000000000000, 0.9330127018922187432, 0.9330127018922192983 ) ) 
 REPRESENTATION_ITEM ( '' )  );
#16760 = ORIENTED_EDGE ( 'NONE', *, *, #6014, .T. ) ;
#16761 = CARTESIAN_POINT ( 'NONE',  ( 85.15643035625001289, -30.70312499938548711, 99.99999999999998579 ) ) ;
#16762 = VECTOR ( 'NONE', #6517, 1000.000000000000000 ) ;
#16763 = CARTESIAN_POINT ( 'NONE',  ( -82.40000000000001990, -33.20624999877097849, 97.00000000000000000 ) ) ;
#16764 = SURFACE_STYLE_FILL_AREA ( #12175 ) ;
#16765 = CARTESIAN_POINT ( 'NONE',  ( -83.77821517812500929, -34.67812499938548854, 102.3871387122750889 ) ) ;
#16766 = PLANE ( 'NONE',  #15868 ) ;
#16767 = EDGE_LOOP ( 'NONE', ( #9333, #3519, #491, #16862, #3299, #2133 ) ) ;
#16768 = EDGE_CURVE ( 'NONE', #1370, #2004, #743, .T. ) ;
#16769 = CARTESIAN_POINT ( 'NONE',  ( -80.90000000000000568, -30.30000000000000426, -97.40192378864668399 ) ) ;
#16770 = EDGE_CURVE ( 'NONE', #11737, #18266, #2392, .T. ) ;
#16771 = CARTESIAN_POINT ( 'NONE',  ( 94.79999999999995453, -35.00000000000000000, 150.0000000000000000 ) ) ;
#16772 = CARTESIAN_POINT ( 'NONE',  ( -4.211140560182196957, -2.431303136016552013, -3.745885042887436178 ) ) ;
#16773 = CARTESIAN_POINT ( 'NONE',  ( 0.000000000000000000, -3.031088913245531202, 1.750000000000006661 ) ) ;
#16774 = EDGE_CURVE ( 'NONE', #13752, #17401, #8361, .T. ) ;
#16775 = CARTESIAN_POINT ( 'NONE',  ( 233.4038475772933623, -32.77634618820330559, -53.00000000000010658 ) ) ;
#16776 = CARTESIAN_POINT ( 'NONE',  ( 229.8435696437499018, -35.22676555956767430, 98.99674139749697588 ) ) ;
#16777 = CARTESIAN_POINT ( 'NONE',  ( -82.39999999999999147, -33.43518749875868679, 103.4641016151377499 ) ) ;
#16778 = AXIS2_PLACEMENT_3D ( 'NONE', #13584, #12131, #14664 ) ;
#16779 = VERTEX_POINT ( 'NONE', #2489 ) ;
#16780 = DIRECTION ( 'NONE',  ( -6.308085367188448025E-15, 0.000000000000000000, -1.000000000000000000 ) ) ;
#16781 = LINE ( 'NONE', #9346, #7274 ) ;
#16782 = CARTESIAN_POINT ( 'NONE',  ( 82.39999999999999147, -34.52812499938548285, 96.81714838363319586 ) ) ;
#16783 = FACE_OUTER_BOUND ( 'NONE', #336, .T. ) ;
#16784 = DIRECTION ( 'NONE',  ( 0.000000000000000000, 0.000000000000000000, 1.000000000000000000 ) ) ;
#16785 = CARTESIAN_POINT ( 'NONE',  ( 83.90000000000000568, -34.96874999877096712, -97.40192378864668399 ) ) ;
#16786 = VECTOR ( 'NONE', #16864, 1000.000000000000000 ) ;
#16787 = FACE_OUTER_BOUND ( 'NONE', #9569, .T. ) ;
#16788 = AXIS2_PLACEMENT_3D ( 'NONE', #9017, #13413, #3146 ) ;
#16789 =( BOUNDED_CURVE ( )  B_SPLINE_CURVE ( 2, ( #15705, #6622, #12571, #11004, #7981, #18443, #6430, #18738, #17069 ),
 .UNSPECIFIED., .F., .F. ) 
 B_SPLINE_CURVE_WITH_KNOTS ( ( 3, 2, 2, 2, 3 ),
 ( 0.5625000000000000000, 0.5694444444444444198, 0.5833333333333333703, 0.5972222222222222099, 0.6041666666666666297 ),
 .UNSPECIFIED. ) 
 CURVE ( )  GEOMETRIC_REPRESENTATION_ITEM ( )  RATIONAL_B_SPLINE_CURVE ( ( 0.9330127018922194093, 0.9330127018922194093, 1.000000000000000000, 0.8660254037844387076, 1.000000000000000000, 0.8660254037844387076, 1.000000000000000000, 0.9330127018922198534, 0.9330127018922192983 ) ) 
 REPRESENTATION_ITEM ( '' )  );
#16790 = VERTEX_POINT ( 'NONE', #8446 ) ;
#16791 = CARTESIAN_POINT ( 'NONE',  ( 232.5999999999999943, -32.16562499938547859, -53.18285161636690361 ) ) ;
#16792 = DIRECTION ( 'NONE',  ( 1.838537592755934481E-31, 0.9242245927363030855, 0.3818493186865927203 ) ) ;
#16793 = ADVANCED_FACE ( 'NONE', ( #10115, #8636 ), #11481, .T. ) ;
#16794 = CARTESIAN_POINT ( 'NONE',  ( 229.8435696437499871, -31.64062499938547290, 98.40857419181659793 ) ) ;
#16795 = CARTESIAN_POINT ( 'NONE',  ( 231.0999999999999375, -34.96874999877096002, -52.59807621135342970 ) ) ;
#16796 = CARTESIAN_POINT ( 'NONE',  ( 3.951447005078451813, 2.357513599190969700, -2.916666666666668295 ) ) ;
#16797 = VECTOR ( 'NONE', #2586, 1000.000000000000000 ) ;
#16798 = ORIENTED_EDGE ( 'NONE', *, *, #290, .T. ) ;
#16799 = VERTEX_POINT ( 'NONE', #13039 ) ;
#16800 = CARTESIAN_POINT ( 'NONE',  ( 232.5999999999999659, -32.53124999877096712, -47.00000000000011369 ) ) ;
#16801 = LINE ( 'NONE', #10831, #10976 ) ;
#16802 = CARTESIAN_POINT ( 'NONE',  ( -83.90000000000000568, -34.12500000000000000, -102.5980762113533018 ) ) ;
#16803 = ORIENTED_EDGE ( 'NONE', *, *, #7100, .F. ) ;
#16804 = CARTESIAN_POINT ( 'NONE',  ( -85.40000000000000568, -31.25624999877096855, 101.7320508075688821 ) ) ;
#16805 = CARTESIAN_POINT ( 'NONE',  ( -83.90000000000000568, -34.36874999877097281, -97.40192378864668399 ) ) ;
#16806 = CONICAL_SURFACE ( 'NONE', #6829, 5.371010071662833063, 1.221730476396037490 ) ;
#16807 = CARTESIAN_POINT ( 'NONE',  ( 82.40000000000000568, -30.00000000000000355, -103.0000000000000000 ) ) ;
#16808 = CARTESIAN_POINT ( 'NONE',  ( -79.39999999999999147, -32.38124999877096855, 98.26794919243110371 ) ) ;
#16809 = EDGE_CURVE ( 'NONE', #5083, #18944, #8125, .T. ) ;
#16810 = CARTESIAN_POINT ( 'NONE',  ( -79.39999999999999147, -33.80624999877097281, 101.7320508075688537 ) ) ;
#16811 = DIRECTION ( 'NONE',  ( 0.000000000000000000, -1.000000000000000000, 0.000000000000000000 ) ) ;
#16812 = CARTESIAN_POINT ( 'NONE',  ( 235.5999999999999943, -32.38124999877096144, 98.26794919243110371 ) ) ;
#16813 =( NAMED_UNIT ( * ) SI_UNIT ( $, .STERADIAN. ) SOLID_ANGLE_UNIT ( ) );
#16814 = DIRECTION ( 'NONE',  ( -0.000000000000000000, -1.000000000000000000, -0.000000000000000000 ) ) ;
#16815 = CARTESIAN_POINT ( 'NONE',  ( 235.3564303562499447, -34.00312499938547717, 101.5914258081833879 ) ) ;
#16816 = CARTESIAN_POINT ( 'NONE',  ( 233.9782151781249411, -31.34062499938548285, 102.3871387122750889 ) ) ;
#16817 = ORIENTED_EDGE ( 'NONE', *, *, #2668, .F. ) ;
#16818 =( NAMED_UNIT ( * ) PLANE_ANGLE_UNIT ( ) SI_UNIT ( $, .RADIAN. ) );
#16819 = EDGE_CURVE ( 'NONE', #13951, #16293, #7180, .T. ) ;
#16820 = CARTESIAN_POINT ( 'NONE',  ( 232.5999999999999375, -31.63124999877096144, 103.4641016151377499 ) ) ;
#16821 = PRODUCT_RELATED_PRODUCT_CATEGORY ( 'part', '', ( #11388 ) ) ;
#16822 = CARTESIAN_POINT ( 'NONE',  ( -82.40000000000000568, -30.00000000000000355, 103.0000000000000000 ) ) ;
#16823 = ORIENTED_EDGE ( 'NONE', *, *, #111, .F. ) ;
#16824 = FACE_BOUND ( 'NONE', #17286, .T. ) ;
#16825 = FACE_OUTER_BOUND ( 'NONE', #6813, .T. ) ;
#16826 = CARTESIAN_POINT ( 'NONE',  ( 84.28136653320187577, -32.00000000000000000, -97.98546077809228905 ) ) ;
#16827 = ORIENTED_EDGE ( 'NONE', *, *, #11389, .F. ) ;
#16828 = CARTESIAN_POINT ( 'NONE',  ( 229.8435696437499871, -34.22812499938547148, -51.59142580818350865 ) ) ;
#16829 = ORIENTED_EDGE ( 'NONE', *, *, #14963, .F. ) ;
#16830 = EDGE_LOOP ( 'NONE', ( #10987, #5139, #19084, #5796 ) ) ;
#16831 = CARTESIAN_POINT ( 'NONE',  ( -81.68701737470171054, -32.00000000000000000, 102.8119722220549903 ) ) ;
#16832 = CARTESIAN_POINT ( 'NONE',  ( 79.64356964375001269, -34.90312499938548285, -101.5914258081833879 ) ) ;
#16833 = CARTESIAN_POINT ( 'NONE',  ( 69.99999999999998579, -34.99999999999999289, -150.0000000000000000 ) ) ;
#16834 =( BOUNDED_CURVE ( )  B_SPLINE_CURVE ( 2, ( #9319, #10978, #3263, #3559, #7766, #360, #9416, #9517, #9622 ),
 .UNSPECIFIED., .F., .F. ) 
 B_SPLINE_CURVE_WITH_KNOTS ( ( 3, 2, 2, 2, 3 ),
 ( 0.8541666666666668517, 0.8611111111111111605, 0.8750000000000000000, 0.8888888888888888395, 0.8958333333333332593 ),
 .UNSPECIFIED. ) 
 CURVE ( )  GEOMETRIC_REPRESENTATION_ITEM ( )  RATIONAL_B_SPLINE_CURVE ( ( 0.9330127018922194093, 0.9330127018922209636, 1.000000000000000000, 0.8660254037844387076, 1.000000000000000000, 0.8660254037844387076, 1.000000000000000000, 0.9330127018922198534, 0.9330127018922192983 ) ) 
 REPRESENTATION_ITEM ( '' )  );
#16835 = CARTESIAN_POINT ( 'NONE',  ( -79.39999999999999147, -33.31874999877096855, 99.99999999999998579 ) ) ;
#16836 = LINE ( 'NONE', #3442, #8362 ) ;
#16837 = CARTESIAN_POINT ( 'NONE',  ( 0.03027795055833683302, 0.6888063905328593028, -3.499999999999998224 ) ) ;
#16838 = CARTESIAN_POINT ( 'NONE',  ( 85.15643035625001289, -32.50312499938548427, -99.99999999999998579 ) ) ;
#16839 = CARTESIAN_POINT ( 'NONE',  ( 79.68063642052044315, -32.00000000000000711, -98.73478688827491112 ) ) ;
#16840 = CARTESIAN_POINT ( 'NONE',  ( -81.02178482187500208, -33.59062499938548285, 102.3871387122750889 ) ) ;
#16841 = CARTESIAN_POINT ( 'NONE',  ( 83.77821517812500929, -34.26562499938548711, -97.61286128772489690 ) ) ;
#16842 = ORIENTED_EDGE ( 'NONE', *, *, #4396, .F. ) ;
#16843 = CARTESIAN_POINT ( 'NONE',  ( 234.0999999999999375, -31.64999999999999858, -47.40192378864679768 ) ) ;
#16844 = FILL_AREA_STYLE_COLOUR ( '', #18320 ) ;
#16845 = CARTESIAN_POINT ( 'NONE',  ( -83.20384757729335945, -34.08615380933863293, 96.99999999999998579 ) ) ;
#16846 = CARTESIAN_POINT ( 'NONE',  ( 235.3564303562499447, -32.27812499938548285, 99.99999999999998579 ) ) ;
#16847 = CARTESIAN_POINT ( 'NONE',  ( -85.15643035624999868, -32.54062499938548569, 98.40857419181659793 ) ) ;
#16848 = CARTESIAN_POINT ( 'NONE',  ( 233.9782151781249411, -32.35312499938547859, -47.61286128772501769 ) ) ;
#16849 = CARTESIAN_POINT ( 'NONE',  ( -85.40000000000000568, -33.11250000000000426, 101.7320508075688679 ) ) ;
#16850 = VERTEX_POINT ( 'NONE', #14493 ) ;
#16851 = DIRECTION ( 'NONE',  ( -1.387778780781445676E-15, -1.000000000000000000, -0.000000000000000000 ) ) ;
#16852 = CARTESIAN_POINT ( 'NONE',  ( 81.28488860390720561, -34.99999999999999289, 97.47285052570519781 ) ) ;
#16853 = CARTESIAN_POINT ( 'NONE',  ( 81.02178482187500208, -32.69062499938548427, 97.61286128772489690 ) ) ;
#16854 = DIRECTION ( 'NONE',  ( -0.000000000000000000, -0.000000000000000000, 1.000000000000000000 ) ) ;
#16855 = CARTESIAN_POINT ( 'NONE',  ( -83.77821517812500929, -31.52812499938548996, 102.3871387122750889 ) ) ;
#16856 = CARTESIAN_POINT ( 'NONE',  ( 0.000000000000000000, 0.000000000000000000, -4.974599999999998801 ) ) ;
#16857 = CARTESIAN_POINT ( 'NONE',  ( 82.39999999999999147, -34.86562499938548854, 103.1828516163667899 ) ) ;
#16858 = CARTESIAN_POINT ( 'NONE',  ( 83.77821517812500929, -30.77812499938548640, -97.61286128772489690 ) ) ;
#16859 = CARTESIAN_POINT ( 'NONE',  ( 231.2217848218749339, -30.96562499938547930, -47.61286128772501769 ) ) ;
#16860 = CARTESIAN_POINT ( 'NONE',  ( -83.77821517812500929, -33.02812499938548285, 97.61286128772489690 ) ) ;
#16861 = CARTESIAN_POINT ( 'NONE',  ( -79.64356964375001269, -34.56562499938549138, -98.40857419181659793 ) ) ;
#16862 = ORIENTED_EDGE ( 'NONE', *, *, #645, .F. ) ;
#16863 = CARTESIAN_POINT ( 'NONE',  ( 85.15643035625001289, -33.40312499938548285, 99.99999999999998579 ) ) ;
#16864 = DIRECTION ( 'NONE',  ( 1.000000000000000000, -0.000000000000000000, -2.407412430484046130E-31 ) ) ;
#16865 = CARTESIAN_POINT ( 'NONE',  ( -83.77821517812500929, -32.01562499938548001, 97.61286128772489690 ) ) ;
#16866 = CARTESIAN_POINT ( 'NONE',  ( -83.77821517812500929, -33.47812499938548569, 97.61286128772489690 ) ) ;
#16867 = CARTESIAN_POINT ( 'NONE',  ( 83.90000000000000568, -33.16874999877096286, 102.5980762113533018 ) ) ;
#16868 = ORIENTED_EDGE ( 'NONE', *, *, #18852, .T. ) ;
#16869 = CARTESIAN_POINT ( 'NONE',  ( -79.39999999999999147, -33.78750000000000142, -101.7320508075688821 ) ) ;
#16870 = EDGE_CURVE ( 'NONE', #13568, #1894, #2726, .T. ) ;
#16871 = EDGE_CURVE ( 'NONE', #2550, #3433, #15967, .T. ) ;
#16872 = CYLINDRICAL_SURFACE ( 'NONE', #2254, 3.000000000000002665 ) ;
#16873 = CARTESIAN_POINT ( 'NONE',  ( 83.20384757729337366, -34.80134618820331127, -103.0000000000000000 ) ) ;
#16874 = CARTESIAN_POINT ( 'NONE',  ( -80.90000000000000568, -32.79374999877096997, 97.40192378864668399 ) ) ;
#16875 = CARTESIAN_POINT ( 'NONE',  ( 229.8435696437499303, -34.30312499938548143, 99.99999999999998579 ) ) ;
#16876 = CARTESIAN_POINT ( 'NONE',  ( -79.39999999999999147, -33.81018749875868679, 101.7320508075688537 ) ) ;
#16877 = EDGE_LOOP ( 'NONE', ( #7541, #9286, #6202, #14937, #3720 ) ) ;
#16878 = CARTESIAN_POINT ( 'NONE',  ( 232.5999999999999375, -34.78124999877096002, 102.9999999999999858 ) ) ;
#16879 = CARTESIAN_POINT ( 'NONE',  ( -83.90000000000000568, -34.36874999877097281, 102.5980762113533018 ) ) ;
#16880 = DIRECTION ( 'NONE',  ( 1.000000000000000000, 0.000000000000000000, -0.000000000000000000 ) ) ;
#16881 = CARTESIAN_POINT ( 'NONE',  ( 85.40000000000000568, -34.48124999877096997, -98.26794919243111792 ) ) ;
#16882 =( BOUNDED_CURVE ( )  B_SPLINE_CURVE ( 2, ( #3416, #14059, #4892, #5086, #15240, #693, #3704, #12209, #7812 ),
 .UNSPECIFIED., .F., .F. ) 
 B_SPLINE_CURVE_WITH_KNOTS ( ( 3, 2, 2, 2, 3 ),
 ( 0.7708333333333333703, 0.7777777777777777901, 0.7916666666666666297, 0.8055555555555555802, 0.8125000000000000000 ),
 .UNSPECIFIED. ) 
 CURVE ( )  GEOMETRIC_REPRESENTATION_ITEM ( )  RATIONAL_B_SPLINE_CURVE ( ( 0.9330127018922192983, 0.9330127018922198534, 1.000000000000000000, 0.8660254037844387076, 1.000000000000000000, 0.8660254037844387076, 1.000000000000000000, 0.9330127018922194093, 0.9330127018922194093 ) ) 
 REPRESENTATION_ITEM ( '' )  );
#16883 = DIRECTION ( 'NONE',  ( 1.000000000000000000, 0.000000000000000000, 0.000000000000000000 ) ) ;
#16884 = CARTESIAN_POINT ( 'NONE',  ( 85.15643035625001289, -32.50312499938548427, -99.99999999999998579 ) ) ;
#16885 = CARTESIAN_POINT ( 'NONE',  ( 230.5523683116323355, -32.00000000000000000, -48.15470523285603832 ) ) ;
#16886 = EDGE_CURVE ( 'NONE', #2507, #12906, #11765, .T. ) ;
#16887 = EDGE_LOOP ( 'NONE', ( #9434, #19130, #13013, #10549 ) ) ;
#16888 = CARTESIAN_POINT ( 'NONE',  ( 231.2217848218749339, -34.82812499938548001, -52.38713871227520968 ) ) ;
#16889 = DIRECTION ( 'NONE',  ( 0.000000000000000000, 0.000000000000000000, 1.000000000000000000 ) ) ;
#16890 = CARTESIAN_POINT ( 'NONE',  ( 235.3564303562499447, -31.86562499938547788, 101.5914258081833879 ) ) ;
#16891 = EDGE_CURVE ( 'NONE', #12136, #12007, #17094, .T. ) ;
#16892 = CARTESIAN_POINT ( 'NONE',  ( 232.5999999999999375, -30.81562499938547717, -53.18285161636690361 ) ) ;
#16893 = CARTESIAN_POINT ( 'NONE',  ( -82.39999999999999147, -33.40312499938548285, 96.81714838363319586 ) ) ;
#16894 = CARTESIAN_POINT ( 'NONE',  ( -82.40000000000000568, -33.03750000000000142, 102.9999999999999858 ) ) ;
#16895 = EDGE_LOOP ( 'NONE', ( #10829, #8787, #2252, #5886, #12025 ) ) ;
#16896 = ORIENTED_EDGE ( 'NONE', *, *, #913, .T. ) ;
#16897 = CARTESIAN_POINT ( 'NONE',  ( -79.79868554281844695, -32.00000000000000711, 98.52838665780579674 ) ) ;
#16898 = CARTESIAN_POINT ( 'NONE',  ( -80.90000000000000568, -33.69374999877096855, -102.5980762113533018 ) ) ;
#16899 = LINE ( 'NONE', #13567, #10977 ) ;
#16900 = ORIENTED_EDGE ( 'NONE', *, *, #1156, .F. ) ;
#16901 = CARTESIAN_POINT ( 'NONE',  ( 79.64356964374998427, -32.24062499938548854, 101.5914258081833879 ) ) ;
#16902 = CARTESIAN_POINT ( 'NONE',  ( -85.40000000000000568, -33.13124999877096855, -101.7320508075688679 ) ) ;
#16903 = DIRECTION ( 'NONE',  ( -0.000000000000000000, -1.000000000000000000, -0.000000000000000000 ) ) ;
#16904 = CARTESIAN_POINT ( 'NONE',  ( -80.90000000000000568, -32.94374999877096855, 102.5980762113533018 ) ) ;
#16905 = CARTESIAN_POINT ( 'NONE',  ( -83.90000000000000568, -33.01874999877097139, 102.5980762113533018 ) ) ;
#16906 = CARTESIAN_POINT ( 'NONE',  ( 234.0999999999999375, -32.34374999877096002, 97.40192378864668399 ) ) ;
#16907 = CARTESIAN_POINT ( 'NONE',  ( 233.3129826252977637, -32.00000000000000000, 102.8119722220550898 ) ) ;
#16908 = CARTESIAN_POINT ( 'NONE',  ( 229.8435696437499871, -33.77812499938548285, 98.40857419181659793 ) ) ;
#16909 = ORIENTED_EDGE ( 'NONE', *, *, #10312, .T. ) ;
#16910 = SHAPE_REPRESENTATION_RELATIONSHIP ( 'NONE' , 'NONE' ,  #7749, #16702 ) ;
#16911 = CARTESIAN_POINT ( 'NONE',  ( 235.5999999999999375, -30.61874999877096215, 99.99999999999998579 ) ) ;
#16912 = CARTESIAN_POINT ( 'NONE',  ( -79.39999999999999147, -32.86874999877097281, -99.99999999999998579 ) ) ;
#16913 = ORIENTED_EDGE ( 'NONE', *, *, #27, .F. ) ;
#16914 = CARTESIAN_POINT ( 'NONE',  ( 113.0000000000000000, 5.199999999999947775, 50.00000000000001421 ) ) ;
#16915 = CARTESIAN_POINT ( 'NONE',  ( -1.840441912298296046E-29, -3.702689427376452761E-13, -103.0000000000001137 ) ) ;
#16916 = CARTESIAN_POINT ( 'NONE',  ( 3.951447005078450925, 2.357513599190970144, 2.916666666666667407 ) ) ;
#16917 = ORIENTED_EDGE ( 'NONE', *, *, #16183, .F. ) ;
#16918 = CARTESIAN_POINT ( 'NONE',  ( 94.79999999999995453, -5.200000000000000178, 150.0000000000000000 ) ) ;
#16919 = AXIS2_PLACEMENT_3D ( 'NONE', #9757, #2710, #2326 ) ;
#16920 = CLOSED_SHELL ( 'NONE', ( #11704, #6782, #5545, #18323, #15576, #10770, #13307 ) ) ;
#16921 = EDGE_LOOP ( 'NONE', ( #8352, #11768, #4591, #5988 ) ) ;
#16922 = ORIENTED_EDGE ( 'NONE', *, *, #12697, .F. ) ;
#16923 = CARTESIAN_POINT ( 'NONE',  ( 79.39999999999999147, -33.35624999877096997, -101.7320508075688537 ) ) ;
#16924 = CARTESIAN_POINT ( 'NONE',  ( 80.90000000000000568, -30.15000000000000213, -97.40192378864668399 ) ) ;
#16925 = FACE_OUTER_BOUND ( 'NONE', #6703, .T. ) ;
#16926 = CARTESIAN_POINT ( 'NONE',  ( -83.90000000000000568, -34.96874999877096712, 97.40192378864668399 ) ) ;
#16927 = EDGE_CURVE ( 'NONE', #7532, #16539, #5367, .T. ) ;
#16928 = CARTESIAN_POINT ( 'NONE',  ( -79.39999999999999147, -33.31874999877096855, 99.99999999999998579 ) ) ;
#16929 = CARTESIAN_POINT ( 'NONE',  ( -2.345747346278108214, 3.264484291692489215, -0.01223254789873409049 ) ) ;
#16930 = CARTESIAN_POINT ( 'NONE',  ( 82.39999999999999147, -33.96562499938548285, -96.81714838363319586 ) ) ;
#16931 = CARTESIAN_POINT ( 'NONE',  ( -79.64356964375001269, -33.55312499938548854, 101.5914258081833879 ) ) ;
#16932 = VECTOR ( 'NONE', #2236, 1000.000000000000000 ) ;
#16933 = VECTOR ( 'NONE', #15191, 1000.000000000000000 ) ;
#16934 = CARTESIAN_POINT ( 'NONE',  ( 83.77821517812500929, -34.56562499938548427, -102.3871387122750889 ) ) ;
#16935 = ORIENTED_EDGE ( 'NONE', *, *, #19056, .F. ) ;
#16936 = CARTESIAN_POINT ( 'NONE',  ( 229.5999999999999375, -31.83749999999999858, -51.73205080756898866 ) ) ;
#16937 = CARTESIAN_POINT ( 'NONE',  ( -85.40000000000000568, -34.46249999999999858, 101.7320508075688679 ) ) ;
#16938 = CARTESIAN_POINT ( 'NONE',  ( 229.8435696437499587, -32.09062499938548285, 98.40857419181659793 ) ) ;
#16939 = CARTESIAN_POINT ( 'NONE',  ( -85.15643035625001289, -31.60312499938548569, 99.99999999999998579 ) ) ;
#16940 = CARTESIAN_POINT ( 'NONE',  ( 232.5999999999999375, -33.06562499938547717, -53.18285161636690361 ) ) ;
#16941 = CARTESIAN_POINT ( 'NONE',  ( -79.39999999999999147, -32.96250000000000568, 101.7320508075688537 ) ) ;
#16942 = EDGE_LOOP ( 'NONE', ( #12201, #5472, #15158, #7726 ) ) ;
#16943 = CARTESIAN_POINT ( 'NONE',  ( 111.0000000000000000, 10.19999999999997620, -137.3499999999999943 ) ) ;
#16944 = ADVANCED_BREP_SHAPE_REPRESENTATION ( '', ( #1092, #10540 ), #12052 ) ;
#16945 = CARTESIAN_POINT ( 'NONE',  ( -81.59615242270662350, -34.76115380933863719, 103.0000000000000000 ) ) ;
#16946 = CARTESIAN_POINT ( 'NONE',  ( 79.64356964374999848, -32.61562499938548854, 99.99999999999998579 ) ) ;
#16947 = CARTESIAN_POINT ( 'NONE',  ( 84.41281071784439405, -31.99999999999999289, -98.10821574224553387 ) ) ;
#16948 = CARTESIAN_POINT ( 'NONE',  ( -85.15643035625001289, -32.05312499938548854, 99.99999999999998579 ) ) ;
#16949 = CARTESIAN_POINT ( 'NONE',  ( 244.7999999999999545, -32.00000000000000000, -100.0000000000000000 ) ) ;
#16950 = CARTESIAN_POINT ( 'NONE',  ( 79.64356964374999848, -34.07812499938548711, 99.99999999999998579 ) ) ;
#16951 = CARTESIAN_POINT ( 'NONE',  ( 79.64356964374999848, -32.72812499938548569, -99.99999999999998579 ) ) ;
#16952 = CARTESIAN_POINT ( 'NONE',  ( 229.8435696437499871, -31.45312499938547290, -48.40857419181671162 ) ) ;
#16953 = CARTESIAN_POINT ( 'NONE',  ( -81.02178482187500208, -33.55312499938548854, 97.61286128772489690 ) ) ;
#16954 = CARTESIAN_POINT ( 'NONE',  ( -85.15643035625001289, -34.75312499938548427, -99.99999999999998579 ) ) ;
#16955 = ORIENTED_EDGE ( 'NONE', *, *, #13303, .F. ) ;
#16956 = CARTESIAN_POINT ( 'NONE',  ( 83.77821517812500929, -32.57812499938548711, 102.3871387122750889 ) ) ;
#16957 = ADVANCED_FACE ( 'NONE', ( #9119 ), #14790, .F. ) ;
#16958 = CYLINDRICAL_SURFACE ( 'NONE', #5876, 2.199999999999993516 ) ;
#16959 = CARTESIAN_POINT ( 'NONE',  ( -83.77821517812500929, -31.41562499938548569, 102.3871387122750889 ) ) ;
#16960 = CARTESIAN_POINT ( 'NONE',  ( -81.02178482187500208, -34.60312499938549280, 102.3871387122750889 ) ) ;
#16961 = CARTESIAN_POINT ( 'NONE',  ( -2.688821387764050996E-14, -4.618802153517012954, -0.4999999999999995559 ) ) ;
#16962 = ORIENTED_EDGE ( 'NONE', *, *, #7911, .F. ) ;
#16963 = CARTESIAN_POINT ( 'NONE',  ( -79.39999999999999147, -33.37500000000000000, -99.99999999999998579 ) ) ;
#16964 = CYLINDRICAL_SURFACE ( 'NONE', #18791, 2.100000000000000089 ) ;
#16965 = LINE ( 'NONE', #3577, #13890 ) ;
#16966 = DIRECTION ( 'NONE',  ( -1.000000000000000000, 4.625929269271494788E-16, 0.000000000000000000 ) ) ;
#16967 = CARTESIAN_POINT ( 'NONE',  ( 233.9782151781249411, -34.15312499938547575, 102.3871387122750889 ) ) ;
#16968 = CARTESIAN_POINT ( 'NONE',  ( -79.39999999999999147, -35.16018749875868821, 101.7320508075688537 ) ) ;
#16969 = ORIENTED_EDGE ( 'NONE', *, *, #7530, .F. ) ;
#16970 = CARTESIAN_POINT ( 'NONE',  ( 229.5999999999999375, -32.69999999999999574, 99.99999999999998579 ) ) ;
#16971 = DIRECTION ( 'NONE',  ( -0.000000000000000000, -0.000000000000000000, -1.000000000000000000 ) ) ;
#16972 = CARTESIAN_POINT ( 'NONE',  ( 229.8848725447336392, -31.99999999999997158, 100.5952676699192381 ) ) ;
#16973 = CARTESIAN_POINT ( 'NONE',  ( -82.40000000000000568, -30.00000000000000355, -103.0000000000000000 ) ) ;
#16974 = CARTESIAN_POINT ( 'NONE',  ( 0.3126073911696412022, -2.020725942163688504, 3.500000000000000444 ) ) ;
#16975 = CARTESIAN_POINT ( 'NONE',  ( 81.02178482187500208, -31.75312499938548427, -97.61286128772489690 ) ) ;
#16976 = CARTESIAN_POINT ( 'NONE',  ( 4.124214193018024943, 2.028338413290970088, 3.513185186763604140 ) ) ;
#16977 = ORIENTED_EDGE ( 'NONE', *, *, #4961, .T. ) ;
#16978 = CARTESIAN_POINT ( 'NONE',  ( 79.39999999999999147, -31.51874999877096784, 99.99999999999998579 ) ) ;
#16979 = DIRECTION ( 'NONE',  ( 1.000000000000000000, 0.000000000000000000, 0.000000000000000000 ) ) ;
#16980 = CARTESIAN_POINT ( 'NONE',  ( 231.2217848218749339, -31.97812499938548214, 102.3871387122750889 ) ) ;
#16981 = CARTESIAN_POINT ( 'NONE',  ( 235.3564303562499447, -31.79062499938547859, -51.59142580818350865 ) ) ;
#16982 = CARTESIAN_POINT ( 'NONE',  ( -85.15643035624999868, -34.15312499938548285, 101.5914258081833879 ) ) ;
#16983 = CARTESIAN_POINT ( 'NONE',  ( -79.64356964374999848, -34.86562499938548143, 99.99999999999998579 ) ) ;
#16984 = ORIENTED_EDGE ( 'NONE', *, *, #9884, .T. ) ;
#16985 = VERTEX_POINT ( 'NONE', #15083 ) ;
#16986 = CARTESIAN_POINT ( 'NONE',  ( -79.64356964375001269, -32.57812499938548001, -101.5914258081833879 ) ) ;
#16987 = CARTESIAN_POINT ( 'NONE',  ( 2.100000000000000089, 0.000000000000000000, -0.2800830152838844622 ) ) ;
#16988 = ORIENTED_EDGE ( 'NONE', *, *, #12448, .F. ) ;
#16989 = CARTESIAN_POINT ( 'NONE',  ( 83.77821517812500929, -33.92812499938548854, 102.3871387122750889 ) ) ;
#16990 = CARTESIAN_POINT ( 'NONE',  ( -82.39999999999999147, -32.98124999877096997, -96.53589838486223584 ) ) ;
#16991 = SHAPE_REPRESENTATION ( 'leg', ( #10540 ), #9915 ) ;
#16992 = CARTESIAN_POINT ( 'NONE',  ( -82.40000000000000568, -33.71249999999998437, 96.99999999999998579 ) ) ;
#16993 = CARTESIAN_POINT ( 'NONE',  ( -83.90000000000000568, -32.71874999877096712, 97.40192378864668399 ) ) ;
#16994 = EDGE_CURVE ( 'NONE', #7775, #8999, #2434, .T. ) ;
#16995 = CARTESIAN_POINT ( 'NONE',  ( -79.39999999999999147, -32.86874999877097281, 99.99999999999998579 ) ) ;
#16996 = CARTESIAN_POINT ( 'NONE',  ( -85.40000000000000568, -32.28750000000000142, 98.26794919243111792 ) ) ;
#16997 = PRODUCT_DEFINITION_SHAPE ( 'NONE', 'NONE',  #15977 ) ;
#16998 = LINE ( 'NONE', #10841, #14253 ) ;
#16999 = CARTESIAN_POINT ( 'NONE',  ( -81.59615242270662350, -34.12634618820329990, 96.99999999999998579 ) ) ;
#17000 = CARTESIAN_POINT ( 'NONE',  ( 232.5999999999999375, -34.30312499938547433, 96.81714838363319586 ) ) ;
#17001 = ADVANCED_FACE ( 'NONE', ( #13517 ), #17828, .F. ) ;
#17002 = ORIENTED_EDGE ( 'NONE', *, *, #8633, .T. ) ;
#17003 = CARTESIAN_POINT ( 'NONE',  ( 79.64356964374999848, -33.06562499938548427, -99.99999999999998579 ) ) ;
#17004 =( NAMED_UNIT ( * ) PLANE_ANGLE_UNIT ( ) SI_UNIT ( $, .RADIAN. ) );
#17005 = CARTESIAN_POINT ( 'NONE',  ( 229.5999999999999375, -30.84374999877096357, 99.99999999999998579 ) ) ;
#17006 = CARTESIAN_POINT ( 'NONE',  ( 229.5999999999999375, -32.19374999877096144, 99.99999999999998579 ) ) ;
#17007 = VERTEX_POINT ( 'NONE', #11956 ) ;
#17008 = CARTESIAN_POINT ( 'NONE',  ( 99.99999999999994316, -35.00000000000000000, 150.0000000000000000 ) ) ;
#17009 = CARTESIAN_POINT ( 'NONE',  ( 0.000000000000000000, 0.000000000000000000, 0.000000000000000000 ) ) ;
#17010 = UNCERTAINTY_MEASURE_WITH_UNIT (LENGTH_MEASURE( 1.000000000000000082E-05 ), #703, 'distance_accuracy_value', 'NONE');
#17011 = DIRECTION ( 'NONE',  ( -1.000000000000000000, 0.000000000000000000, 0.000000000000000000 ) ) ;
#17012 = VERTEX_POINT ( 'NONE', #7272 ) ;
#17013 = DIRECTION ( 'NONE',  ( -1.000000000000000000, 1.586032892321652285E-15, -0.000000000000000000 ) ) ;
#17014 = CARTESIAN_POINT ( 'NONE',  ( 4.071447262713888016, -2.020725942163695166, -3.500000000000000000 ) ) ;
#17015 = ORIENTED_EDGE ( 'NONE', *, *, #2656, .T. ) ;
#17016 = CARTESIAN_POINT ( 'NONE',  ( -79.68596062386970402, -32.00000000000002132, 101.2782762865727619 ) ) ;
#17017 = EDGE_CURVE ( 'NONE', #14982, #16515, #15222, .T. ) ;
#17018 = CARTESIAN_POINT ( 'NONE',  ( 85.40000000000000568, -31.38749999999999574, -98.26794919243111792 ) ) ;
#17019 = CARTESIAN_POINT ( 'NONE',  ( -82.40000000000000568, -30.50624999877097210, 96.99999999999998579 ) ) ;
#17020 = ADVANCED_FACE ( 'NONE', ( #7369 ), #13227, .T. ) ;
#17021 = CARTESIAN_POINT ( 'NONE',  ( -83.90000000000000568, -34.51874999877097139, 97.40192378864668399 ) ) ;
#17022 = CARTESIAN_POINT ( 'NONE',  ( -82.39999999999999147, -33.93356250001229313, 103.4641016151377499 ) ) ;
#17023 = CARTESIAN_POINT ( 'NONE',  ( 83.90000000000000568, -32.17500000000000426, -102.5980762113533018 ) ) ;
#17024 = CARTESIAN_POINT ( 'NONE',  ( 232.5999999999999091, -33.03749999999998721, 102.9999999999999858 ) ) ;
#17025 = ADVANCED_FACE ( 'NONE', ( #8925 ), #17226, .T. ) ;
#17026 = CARTESIAN_POINT ( 'NONE',  ( 83.77821517812500929, -32.57812499938548711, -97.61286128772489690 ) ) ;
#17027 = CARTESIAN_POINT ( 'NONE',  ( 81.59615242270662350, -33.73259618943233562, 102.9999999999999858 ) ) ;
#17028 = CARTESIAN_POINT ( 'NONE',  ( -85.15643035624999868, -34.15312499938548285, 101.5914258081833879 ) ) ;
#17029 = AXIS2_PLACEMENT_3D ( 'NONE', #12860, #15797, #2591 ) ;
#17030 = CARTESIAN_POINT ( 'NONE',  ( 82.39999999999999147, -34.75312499938549138, -96.81714838363319586 ) ) ;
#17031 = ORIENTED_EDGE ( 'NONE', *, *, #6014, .F. ) ;
#17032 = CARTESIAN_POINT ( 'NONE',  ( 80.90000000000000568, -33.00000000000000000, 97.40192378864668399 ) ) ;
#17033 = CARTESIAN_POINT ( 'NONE',  ( -80.90000000000000568, -33.30000000000000426, 97.40192378864668399 ) ) ;
#17034 = CARTESIAN_POINT ( 'NONE',  ( 0.1750025118121568690, 4.719839900820621104, -3.469254087858248070 ) ) ;
#17035 = CARTESIAN_POINT ( 'NONE',  ( 229.5999999999999375, -34.91249999999999432, -48.26794919243123161 ) ) ;
#17036 = CARTESIAN_POINT ( 'NONE',  ( -85.15643035624999868, -31.19062499938548783, 98.40857419181659793 ) ) ;
#17037 = EDGE_CURVE ( 'NONE', #11539, #518, #7464, .T. ) ;
#17038 = CARTESIAN_POINT ( 'NONE',  ( 229.8435696437499303, -32.50312499938547717, -50.00000000000011369 ) ) ;
#17039 = CARTESIAN_POINT ( 'NONE',  ( -79.39999999999999147, -32.47500000000000142, 99.99999999999998579 ) ) ;
#17040 = ORIENTED_EDGE ( 'NONE', *, *, #15091, .F. ) ;
#17041 = CARTESIAN_POINT ( 'NONE',  ( 3.974183935050569882, -0.7239581970533436328, 3.565826011443134380 ) ) ;
#17042 = AXIS2_PLACEMENT_3D ( 'NONE', #5734, #7003, #960 ) ;
#17043 = CARTESIAN_POINT ( 'NONE',  ( 82.39999999999999147, -32.95312499938548711, 103.1828516163667899 ) ) ;
#17044 = CARTESIAN_POINT ( 'NONE',  ( 230.4319669496466076, -32.00000000000000000, -48.28830862702061921 ) ) ;
#17045 = EDGE_CURVE ( 'NONE', #12372, #16126, #11411, .T. ) ;
#17046 = CARTESIAN_POINT ( 'NONE',  ( -79.64356964374999848, -30.92812499938548498, 99.99999999999998579 ) ) ;
#17047 = CARTESIAN_POINT ( 'NONE',  ( -81.02178482187500208, -32.80312499938548854, -97.61286128772489690 ) ) ;
#17048 = CARTESIAN_POINT ( 'NONE',  ( 83.77821517812500929, -32.01562499938548001, 102.3871387122750889 ) ) ;
#17049 =( GEOMETRIC_REPRESENTATION_CONTEXT ( 3 ) GLOBAL_UNCERTAINTY_ASSIGNED_CONTEXT ( ( #1966 ) ) GLOBAL_UNIT_ASSIGNED_CONTEXT ( ( #9972, #2624, #1460 ) ) REPRESENTATION_CONTEXT ( 'NONE', 'WORKASPACE' ) );
#17050 = CARTESIAN_POINT ( 'NONE',  ( 82.39999999999999147, -31.26562499938549067, -96.81714838363319586 ) ) ;
#17051 = CARTESIAN_POINT ( 'NONE',  ( 232.5999999999999375, -34.30312499938547433, -53.18285161636690361 ) ) ;
#17052 = CARTESIAN_POINT ( 'NONE',  ( -82.39999999999999147, -33.74062499938548854, 103.1828516163667899 ) ) ;
#17053 = CARTESIAN_POINT ( 'NONE',  ( -85.15643035625001289, -34.30312499938548854, -99.99999999999998579 ) ) ;
#17054 = VERTEX_POINT ( 'NONE', #15906 ) ;
#17055 = CARTESIAN_POINT ( 'NONE',  ( 79.64356964375001269, -32.69062499938548427, 101.5914258081833879 ) ) ;
#17056 = CARTESIAN_POINT ( 'NONE',  ( 5.100000000000002309, 0.000000000000000000, 5.200000000000001066 ) ) ;
#17057 = CARTESIAN_POINT ( 'NONE',  ( -85.15643035624999868, -31.90312499938548285, 101.5914258081833879 ) ) ;
#17058 = CARTESIAN_POINT ( 'NONE',  ( -79.64356964375001269, -34.56562499938549138, 101.5914258081833879 ) ) ;
#17059 = CARTESIAN_POINT ( 'NONE',  ( 82.39999999999999147, -34.83749999999999858, 97.00000000000000000 ) ) ;
#17060 = ORIENTED_EDGE ( 'NONE', *, *, #16423, .T. ) ;
#17061 = CARTESIAN_POINT ( 'NONE',  ( -85.40000000000000568, -34.46249999999999858, -98.26794919243111792 ) ) ;
#17062 = CARTESIAN_POINT ( 'NONE',  ( 229.5999999999999375, -34.40624999877096002, -48.26794919243123161 ) ) ;
#17063 = CARTESIAN_POINT ( 'NONE',  ( 232.1497501643324881, -35.00000000000000711, -52.97309102824105764 ) ) ;
#17064 = FACE_OUTER_BOUND ( 'NONE', #19230, .T. ) ;
#17065 = CARTESIAN_POINT ( 'NONE',  ( 229.8435696437499871, -31.97812499938548214, 98.40857419181659793 ) ) ;
#17066 = CARTESIAN_POINT ( 'NONE',  ( -82.39999999999999147, -35.23518749875867684, 103.4641016151377499 ) ) ;
#17067 = CARTESIAN_POINT ( 'NONE',  ( 230.7186334667984227, -32.00000000000000711, -52.01453922190813728 ) ) ;
#17068 = CARTESIAN_POINT ( 'NONE',  ( 80.90000000000000568, -32.94374999877096855, -102.5980762113533018 ) ) ;
#17069 = CARTESIAN_POINT ( 'NONE',  ( -82.39999999999999147, -33.65624999877097423, -103.0000000000000000 ) ) ;
#17070 = CARTESIAN_POINT ( 'NONE',  ( 81.02178482187500208, -30.85312499938548569, 102.3871387122750889 ) ) ;
#17071 = CARTESIAN_POINT ( 'NONE',  ( 105.1999999999999744, -34.51168759575591594, -100.0000000000000000 ) ) ;
#17072 = AXIS2_PLACEMENT_3D ( 'NONE', #1489, #10658, #15153 ) ;
#17073 = CARTESIAN_POINT ( 'NONE',  ( 85.15643035625001289, -31.15312499938548996, -99.99999999999998579 ) ) ;
#17074 = FACE_OUTER_BOUND ( 'NONE', #17430, .T. ) ;
#17075 = VERTEX_POINT ( 'NONE', #17566 ) ;
#17076 = CARTESIAN_POINT ( 'NONE',  ( 82.39999999999999147, -31.85624999877097352, 103.4641016151377499 ) ) ;
#17077 = APPLICATION_PROTOCOL_DEFINITION ( 'draft international standard', 'automotive_design', 1998, #4969 ) ;
#17078 = CARTESIAN_POINT ( 'NONE',  ( 229.8435696437499871, -33.36562499938548143, 101.5914258081833879 ) ) ;
#17079 = CARTESIAN_POINT ( 'NONE',  ( 233.9782151781249411, -32.35312499938547859, -47.61286128772501769 ) ) ;
#17080 = STYLED_ITEM ( 'NONE', ( #16530 ), #5537 ) ;
#17081 = CARTESIAN_POINT ( 'NONE',  ( -83.77821517812500929, -34.26562499938548711, 97.61286128772489690 ) ) ;
#17082 = CARTESIAN_POINT ( 'NONE',  ( 244.7999999999999545, -29.80000000000002203, 150.0000000000000000 ) ) ;
#17083 = ORIENTED_EDGE ( 'NONE', *, *, #18438, .F. ) ;
#17084 = ORIENTED_EDGE ( 'NONE', *, *, #13639, .F. ) ;
#17085 = CARTESIAN_POINT ( 'NONE',  ( -79.64356964375001269, -31.30312499938548854, -98.40857419181659793 ) ) ;
#17086 = CARTESIAN_POINT ( 'NONE',  ( -83.20384757729334524, -30.93615380933863079, 96.99999999999997158 ) ) ;
#17087 = ORIENTED_EDGE ( 'NONE', *, *, #3496, .T. ) ;
#17088 = CARTESIAN_POINT ( 'NONE',  ( 79.64356964374998427, -32.76562499938548711, 98.40857419181659793 ) ) ;
#17089 = AXIS2_PLACEMENT_3D ( 'NONE', #10756, #15255, #6663 ) ;
#17090 = CARTESIAN_POINT ( 'NONE',  ( -85.40000000000000568, -32.64374999877097139, -99.99999999999998579 ) ) ;
#17091 = CARTESIAN_POINT ( 'NONE',  ( 85.40000000000000568, -34.08749999999999858, 101.7320508075688679 ) ) ;
#17092 = CARTESIAN_POINT ( 'NONE',  ( -82.39999999999999147, -32.30624999877097281, 96.53589838486223584 ) ) ;
#17093 = CARTESIAN_POINT ( 'NONE',  ( -83.90000000000000568, -34.06874999877096855, 97.40192378864668399 ) ) ;
#17094 = CIRCLE ( 'NONE', #8662, 5.560781378645573980 ) ;
#17095 = CARTESIAN_POINT ( 'NONE',  ( 83.20395887649171129, -35.00000000000000711, -102.6365808225363878 ) ) ;
#17096 = AXIS2_PLACEMENT_3D ( 'NONE', #4918, #5311, #9596 ) ;
#17097 = CARTESIAN_POINT ( 'NONE',  ( 232.1497501643324881, -35.00000000000000711, 97.02690897175904183 ) ) ;
#17098 = CARTESIAN_POINT ( 'NONE',  ( 79.39999999999999147, -30.58124999877096784, -98.26794919243110371 ) ) ;
#17099 = CARTESIAN_POINT ( 'NONE',  ( 232.5999999999999375, -33.40312499938547575, 96.81714838363319586 ) ) ;
#17100 = ORIENTED_EDGE ( 'NONE', *, *, #1136, .T. ) ;
#17101 = CARTESIAN_POINT ( 'NONE',  ( 85.15643035625001289, -33.77812499938548285, -98.40857419181659793 ) ) ;
#17102 = SURFACE_STYLE_USAGE ( .BOTH. , #5095 ) ;
#17103 = CARTESIAN_POINT ( 'NONE',  ( 234.0999999999999375, -31.14374999877096428, 102.5980762113533018 ) ) ;
#17104 = CARTESIAN_POINT ( 'NONE',  ( 84.44763168836730927, -32.00000000000000711, -101.8452947671444093 ) ) ;
#17105 = ORIENTED_EDGE ( 'NONE', *, *, #8093, .T. ) ;
#17106 = CARTESIAN_POINT ( 'NONE',  ( -82.40000000000000568, -30.00000000000000355, 99.99999999999998579 ) ) ;
#17107 = DIRECTION ( 'NONE',  ( -1.000000000000000000, 0.000000000000000000, 0.000000000000000000 ) ) ;
#17108 = DIRECTION ( 'NONE',  ( -0.000000000000000000, -1.000000000000000000, -0.000000000000000000 ) ) ;
#17109 = ORIENTED_EDGE ( 'NONE', *, *, #4755, .T. ) ;
#17110 = CARTESIAN_POINT ( 'NONE',  ( -79.39999999999999147, -32.00624999877096855, 101.7320508075688537 ) ) ;
#17111 = VECTOR ( 'NONE', #8085, 1000.000000000000000 ) ;
#17112 = ADVANCED_FACE ( 'NONE', ( #18939 ), #970, .F. ) ;
#17113 =( BOUNDED_CURVE ( )  B_SPLINE_CURVE ( 2, ( #7288, #2695, #14804, #1624, #13243, #7385, #5832, #9042, #7484 ),
 .UNSPECIFIED., .F., .F. ) 
 B_SPLINE_CURVE_WITH_KNOTS ( ( 3, 2, 2, 2, 3 ),
 ( 0.5625000000000002220, 0.5694444444444444198, 0.5833333333333333703, 0.5972222222222222099, 0.6041666666666667407 ),
 .UNSPECIFIED. ) 
 CURVE ( )  GEOMETRIC_REPRESENTATION_ITEM ( )  RATIONAL_B_SPLINE_CURVE ( ( 0.9330127018922194093, 0.9330127018922215187, 1.000000000000000000, 0.8660254037844387076, 1.000000000000000000, 0.8660254037844387076, 1.000000000000000000, 0.9330127018922187432, 0.9330127018922192983 ) ) 
 REPRESENTATION_ITEM ( '' )  );
#17114 = VECTOR ( 'NONE', #7884, 1000.000000000000000 ) ;
#17115 = CARTESIAN_POINT ( 'NONE',  ( 232.5999999999999375, -32.98124999877095576, 102.9999999999999858 ) ) ;
#17116 = ORIENTED_EDGE ( 'NONE', *, *, #3753, .F. ) ;
#17117 = CARTESIAN_POINT ( 'NONE',  ( 85.40000000000000568, -30.90000000000000213, -99.99999999999998579 ) ) ;
#17118 = CARTESIAN_POINT ( 'NONE',  ( -4.000000000000000000, -1.942223658245633811, -0.3516579909967644246 ) ) ;
#17119 = EDGE_CURVE ( 'NONE', #13429, #14350, #16001, .T. ) ;
#17120 = EDGE_CURVE ( 'NONE', #2466, #9248, #2705, .T. ) ;
#17121 = CARTESIAN_POINT ( 'NONE',  ( -80.90000000000000568, -33.69374999877096855, 97.40192378864668399 ) ) ;
#17122 = CARTESIAN_POINT ( 'NONE',  ( -83.90000000000000568, -30.37500000000000355, 102.5980762113533018 ) ) ;
#17123 = CARTESIAN_POINT ( 'NONE',  ( 233.2908335840014615, -34.99999999999998579, -52.88685016125990046 ) ) ;
#17124 = SURFACE_STYLE_USAGE ( .BOTH. , #11155 ) ;
#17125 = PLANE ( 'NONE',  #8307 ) ;
#17126 = AXIS2_PLACEMENT_3D ( 'NONE', #8654, #13346, #7578 ) ;
#17127 = LINE ( 'NONE', #8134, #18053 ) ;
#17128 = CARTESIAN_POINT ( 'NONE',  ( -81.02178482187500208, -32.09062499938548285, 97.61286128772489690 ) ) ;
#17129 = FACE_BOUND ( 'NONE', #15790, .T. ) ;
#17130 = EDGE_LOOP ( 'NONE', ( #6856, #4986, #9194, #830 ) ) ;
#17131 = CARTESIAN_POINT ( 'NONE',  ( -82.39999999999999147, -33.71249999999999858, 96.53589838486223584 ) ) ;
#17132 = ADVANCED_FACE ( 'NONE', ( #17472 ), #4081, .T. ) ;
#17133 = CYLINDRICAL_SURFACE ( 'NONE', #18966, 3.000000000000009770 ) ;
#17134 = CARTESIAN_POINT ( 'NONE',  ( -85.15643035625001289, -33.40312499938548285, 99.99999999999998579 ) ) ;
#17135 = EDGE_CURVE ( 'NONE', #3211, #6709, #8601, .T. ) ;
#17136 = CARTESIAN_POINT ( 'NONE',  ( 231.2217848218749339, -35.12812499938548427, -47.61286128772501769 ) ) ;
#17137 = ADVANCED_FACE ( 'NONE', ( #16200 ), #9336, .F. ) ;
#17138 = ORIENTED_EDGE ( 'NONE', *, *, #7661, .T. ) ;
#17139 = CARTESIAN_POINT ( 'NONE',  ( 3.958491816110462747, 1.406739583089039902, 3.500000000000000000 ) ) ;
#17140 = DIRECTION ( 'NONE',  ( 0.000000000000000000, 0.000000000000000000, 1.000000000000000000 ) ) ;
#17141 = CARTESIAN_POINT ( 'NONE',  ( 81.02178482187500208, -32.54062499938548569, 102.3871387122750889 ) ) ;
#17142 = CARTESIAN_POINT ( 'NONE',  ( 0.1756481739660539498, -4.720212674038995360, -3.469390959564070620 ) ) ;
#17143 = CARTESIAN_POINT ( 'NONE',  ( 232.5999999999999943, -32.27812499938547575, -46.81714838363331666 ) ) ;
#17144 = CARTESIAN_POINT ( 'NONE',  ( -82.39999999999999147, -34.19062499938548427, 103.1828516163667899 ) ) ;
#17145 = CARTESIAN_POINT ( 'NONE',  ( 5.560781378645575757, 0.000000000000000000, -4.000000000000000000 ) ) ;
#17146 = CARTESIAN_POINT ( 'NONE',  ( 81.02178482187500208, -32.09062499938548285, 102.3871387122750889 ) ) ;
#17147 = CARTESIAN_POINT ( 'NONE',  ( 84.51154815724953551, -35.25364861271051353, -98.22820072003833047 ) ) ;
#17148 = CARTESIAN_POINT ( 'NONE',  ( 233.9782151781249411, -32.99062499938548143, -52.38713871227520968 ) ) ;
#17149 = CARTESIAN_POINT ( 'NONE',  ( -85.15643035625001289, -33.36562499938548854, 101.5914258081833879 ) ) ;
#17150 = CARTESIAN_POINT ( 'NONE',  ( -81.02178482187500208, -31.79062499938548925, -97.61286128772489690 ) ) ;
#17151 = ORIENTED_EDGE ( 'NONE', *, *, #2265, .T. ) ;
#17152 = CARTESIAN_POINT ( 'NONE',  ( 79.64356964374999848, -31.82812499938548356, 99.99999999999998579 ) ) ;
#17153 = CARTESIAN_POINT ( 'NONE',  ( 233.4038475772933623, -32.77634618820330559, 97.00000000000000000 ) ) ;
#17154 = CARTESIAN_POINT ( 'NONE',  ( -79.39999999999999147, -33.33749999999999858, 98.26794919243110371 ) ) ;
#17155 = CARTESIAN_POINT ( 'NONE',  ( -85.15643035624999868, -31.52812499938547930, 98.40857419181659793 ) ) ;
#17156 = CARTESIAN_POINT ( 'NONE',  ( -85.15643035624999868, -34.71562499938548285, 101.5914258081833879 ) ) ;
#17157 = EDGE_CURVE ( 'NONE', #14350, #18754, #1507, .T. ) ;
#17158 = FACE_OUTER_BOUND ( 'NONE', #15323, .T. ) ;
#17159 = ORIENTED_EDGE ( 'NONE', *, *, #4522, .F. ) ;
#17160 = EDGE_CURVE ( 'NONE', #16515, #12559, #2749, .T. ) ;
#17161 = CARTESIAN_POINT ( 'NONE',  ( -79.39999999999999147, -32.47500000000000142, -99.99999999999998579 ) ) ;
#17162 = PRODUCT_DEFINITION_SHAPE ( 'NONE', 'NONE',  #11913 ) ;
#17163 = CARTESIAN_POINT ( 'NONE',  ( 111.0000000000000000, 6.932050807568741924, -134.9680512646005184 ) ) ;
#17164 = CARTESIAN_POINT ( 'NONE',  ( 232.5999999999999375, -34.16249999999999432, -53.00000000000010658 ) ) ;
#17165 = CARTESIAN_POINT ( 'NONE',  ( -85.40000000000000568, -30.40856250001229455, 101.7320508075688679 ) ) ;
#17166 = CARTESIAN_POINT ( 'NONE',  ( 229.8435696437499303, -31.04062499938547859, 99.99999999999998579 ) ) ;
#17167 = CARTESIAN_POINT ( 'NONE',  ( -85.40000000000000568, -35.37132790096610080, 98.90809659374338025 ) ) ;
#17168 = EDGE_CURVE ( 'NONE', #8568, #6753, #8510, .T. ) ;
#17169 = CARTESIAN_POINT ( 'NONE',  ( 83.20384757729335945, -33.90134618820329848, -102.9999999999999716 ) ) ;
#17170 = CARTESIAN_POINT ( 'NONE',  ( -82.40000000000000568, -34.55624999877097281, 97.00000000000000000 ) ) ;
#17171 = DIRECTION ( 'NONE',  ( 1.000000000000000000, 0.000000000000000000, 0.000000000000000000 ) ) ;
#17172 = CARTESIAN_POINT ( 'NONE',  ( -99.99999999999998579, -29.80000000000000426, 150.0000000000000000 ) ) ;
#17173 = DIRECTION ( 'NONE',  ( 0.000000000000000000, 0.000000000000000000, -1.000000000000000000 ) ) ;
#17174 = LINE ( 'NONE', #3777, #10569 ) ;
#17175 = CARTESIAN_POINT ( 'NONE',  ( 81.02178482187500208, -31.00312499938548783, -102.3871387122750889 ) ) ;
#17176 = CARTESIAN_POINT ( 'NONE',  ( 4.170895651974599438, 2.054890354522711515, 3.559174498016425048 ) ) ;
#17177 = ORIENTED_EDGE ( 'NONE', *, *, #16427, .T. ) ;
#17178 = LINE ( 'NONE', #12389, #12243 ) ;
#17179 = APPLICATION_PROTOCOL_DEFINITION ( 'draft international standard', 'automotive_design', 1998, #6080 ) ;
#17180 = CARTESIAN_POINT ( 'NONE',  ( 232.5999999999999375, -31.94062499938548072, 103.1828516163667899 ) ) ;
#17181 = CARTESIAN_POINT ( 'NONE',  ( 235.3564303562499447, -33.14062499938548001, -51.59142580818350865 ) ) ;
#17182 = CARTESIAN_POINT ( 'NONE',  ( -81.02178482187500208, -33.89062499938548711, 97.61286128772489690 ) ) ;
#17183 = CARTESIAN_POINT ( 'NONE',  ( 82.40000000000000568, -33.93750000000000711, 97.00000000000000000 ) ) ;
#17184 = ORIENTED_EDGE ( 'NONE', *, *, #5306, .T. ) ;
#17185 = CARTESIAN_POINT ( 'NONE',  ( -79.64356964374999848, -32.16562499938548569, -99.99999999999998579 ) ) ;
#17186 = DIRECTION ( 'NONE',  ( 0.000000000000000000, -1.000000000000000000, 0.000000000000000000 ) ) ;
#17187 = ORIENTED_EDGE ( 'NONE', *, *, #15963, .T. ) ;
#17188 = CARTESIAN_POINT ( 'NONE',  ( 81.02178482187500208, -34.45312499938548711, 102.3871387122750889 ) ) ;
#17189 = CARTESIAN_POINT ( 'NONE',  ( -80.90000000000000568, -32.94374999877096855, -97.40192378864668399 ) ) ;
#17190 = CARTESIAN_POINT ( 'NONE',  ( 79.39999999999999147, -34.27499999999999858, 99.99999999999998579 ) ) ;
#17191 = CARTESIAN_POINT ( 'NONE',  ( -83.20384757729335945, -34.40759618943233988, 102.9999999999999858 ) ) ;
#17192 = CARTESIAN_POINT ( 'NONE',  ( -83.90000000000000568, -32.26874999877097139, 97.40192378864668399 ) ) ;
#17193 = CARTESIAN_POINT ( 'NONE',  ( -79.64356964375001269, -31.34062499938548640, 98.40857419181659793 ) ) ;
#17194 = CARTESIAN_POINT ( 'NONE',  ( -85.15643035625001289, -33.74062499938548854, -99.99999999999998579 ) ) ;
#17195 = CARTESIAN_POINT ( 'NONE',  ( 82.40000000000000568, -34.10624999877096997, -96.99999999999998579 ) ) ;
#17196 = CARTESIAN_POINT ( 'NONE',  ( -79.39999999999999147, -34.21874999877096712, 99.99999999999998579 ) ) ;
#17197 = CARTESIAN_POINT ( 'NONE',  ( 229.8435696437499871, -34.15312499938547575, 101.5914258081833879 ) ) ;
#17198 = ORIENTED_EDGE ( 'NONE', *, *, #2420, .T. ) ;
#17199 = CARTESIAN_POINT ( 'NONE',  ( 83.77821517812500929, -32.76562499938548711, -102.3871387122750889 ) ) ;
#17200 = CARTESIAN_POINT ( 'NONE',  ( -85.15643035624999868, -35.05312499938548143, -98.40857419181659793 ) ) ;
#17201 = CARTESIAN_POINT ( 'NONE',  ( 229.5999999999999375, -31.33124999877096073, -51.73205080756898866 ) ) ;
#17202 = EDGE_LOOP ( 'NONE', ( #15149, #253, #12875, #18621 ) ) ;
#17203 = CARTESIAN_POINT ( 'NONE',  ( 231.7961524227065695, -34.40759618943233988, 102.9999999999999858 ) ) ;
#17204 = EDGE_CURVE ( 'NONE', #7647, #2658, #11166, .T. ) ;
#17205 = CARTESIAN_POINT ( 'NONE',  ( -83.77821517812500929, -30.21562499938548285, 97.61286128772489690 ) ) ;
#17206 = CARTESIAN_POINT ( 'NONE',  ( 79.39999999999999147, -32.02500000000000568, 99.99999999999998579 ) ) ;
#17207 = ORIENTED_EDGE ( 'NONE', *, *, #19070, .F. ) ;
#17208 = CARTESIAN_POINT ( 'NONE',  ( 4.158921614371307918, -1.986121848748765073, 3.559936047944508797 ) ) ;
#17209 = CARTESIAN_POINT ( 'NONE',  ( 4.093692494532770176, -2.021783646005775203, 3.501831996793854707 ) ) ;
#17210 = ORIENTED_EDGE ( 'NONE', *, *, #12360, .T. ) ;
#17211 = FILL_AREA_STYLE_COLOUR ( '', #18274 ) ;
#17212 = CARTESIAN_POINT ( 'NONE',  ( 85.40000000000000568, -32.21249999999999858, -101.7320508075688679 ) ) ;
#17213 = CARTESIAN_POINT ( 'NONE',  ( 232.5999999999999375, -32.30624999877096570, 97.00000000000000000 ) ) ;
#17214 = CARTESIAN_POINT ( 'NONE',  ( -82.39999999999999147, -30.81562499938548427, 96.81714838363319586 ) ) ;
#17215 = CARTESIAN_POINT ( 'NONE',  ( -85.40000000000000568, -34.45856250001228460, 101.7320508075688679 ) ) ;
#17216 = UNCERTAINTY_MEASURE_WITH_UNIT (LENGTH_MEASURE( 1.000000000000000082E-05 ), #16424, 'distance_accuracy_value', 'NONE');
#17217 = CARTESIAN_POINT ( 'NONE',  ( -83.90000000000000568, -32.11874999877097281, -97.40192378864668399 ) ) ;
#17218 = CARTESIAN_POINT ( 'NONE',  ( -82.39999999999999147, -34.33124999877097139, 103.0000000000000000 ) ) ;
#17219 = CARTESIAN_POINT ( 'NONE',  ( -81.59615242270665192, -33.28259618943233278, 97.00000000000000000 ) ) ;
#17220 = CARTESIAN_POINT ( 'NONE',  ( -82.39999999999999147, -33.17812499938548854, 103.1828516163667899 ) ) ;
#17221 = CARTESIAN_POINT ( 'NONE',  ( 82.39999999999999147, -34.97812499938547859, -103.1828516163667899 ) ) ;
#17222 = ORIENTED_EDGE ( 'NONE', *, *, #5066, .T. ) ;
#17223 = CARTESIAN_POINT ( 'NONE',  ( 229.5999999999999375, -34.94999999999999574, -50.00000000000011369 ) ) ;
#17224 = CARTESIAN_POINT ( 'NONE',  ( 82.40000000000000568, -30.00000000000000355, -96.99999999999998579 ) ) ;
#17225 = ADVANCED_FACE ( 'NONE', ( #1094 ), #4217, .T. ) ;
#17226 =( BOUNDED_SURFACE ( )  B_SPLINE_SURFACE ( 1, 2, ( 
 ( #15474, #2186, #353, #9312, #16742, #15373, #6299, #3355, #9610, #18409, #1891, #12250, #2086, #13608, #4836, #18218, #10779, #15573, #10969, #12347, #5124, #4738, #6587, #11067, #15276, #17036, #1989, #8042, #3647, #9507, #3551, #536, #12534, #13712, #250, #6207, #16939, #14000, #18506, #7946, #12155, #6492, #10683, #18122, #9210, #16651, #638, #12441, #7849, #3254, #13803, #15176, #1793, #446, #7757, #6393, #13898, #18313, #4932, #5029, #10876, #16847, #3451, #9408, #6971, #18894, #13019, #16050, #12923, #17519, #2557, #18704, #5323, #17428, #14380, #733, #11361, #3740, #9998, #5219, #2471, #3834, #11556, #15954, #17134, #14471, #6881, #12829, #9802, #6787, #14191, #8520, #18796, #1019, #11169, #17230, #5514, #11262, #4132, #7060, #18605, #1102, #9901, #11460, #18991, #5421, #12735, #15864, #8427, #4039, #17326, #15764, #14094, #828, #10092, #2371, #3935, #5612, #8142, #14288, #12631, #6687, #9707, #15668, #2277, #8241, #8332, #924, #2855, #14967, #1303, #8812, #14668, #9006, #7161 ),
 ( #13110, #19177, #4326, #14567, #6085, #4513, #10572, #8714, #17711, #5790, #4418, #7250, #11744, #18003, #7445, #10286, #13205, #10469, #2653, #16246, #14767, #1396, #4616, #34, #7347, #13496, #19080, #1589, #135, #13301, #12032, #10377, #16435, #8616, #17907, #11936, #8902, #7537, #2759, #1204, #5699, #5984, #3044, #11651, #16339, #17611, #14864, #4227, #10183, #16146, #19276, #5892, #11840, #17808, #2948, #1491, #13402, #12485, #589, #18551, #3497, #6539, #12780, #2226, #5076, #9456, #5272, #5368, #7993, #15421, #13949, #18749, #14142, #15521, #8284, #7897, #9752, #14235, #2032, #873, #5166, #11217, #6836, #12677, #6732, #3694, #15716, #16893, #16536, #3136, #776, #18651, #2321, #11113, #9095, #9660, #13847, #15060, #12393, #488, #17182, #15620, #18455, #1936, #11017, #6441, #18361, #16982, #3786, #4983, #17081, #10925, #3594, #8192, #9555, #2138, #8096, #14048, #683, #6635, #12583, #8664, #17372, #14332, #1059, #14425, #17661, #7112, #2511, #10237, #3885, #5655, #8381, #8468, #18845 ) ),
 .UNSPECIFIED., .F., .F., .F. ) 
 B_SPLINE_SURFACE_WITH_KNOTS ( ( 2, 2 ),
 ( 3, 2, 2, 2, 2, 2, 2, 2, 2, 2, 2, 2, 2, 2, 2, 2, 2, 2, 2, 2, 2, 2, 2, 2, 2, 2, 2, 2, 2, 2, 2, 2, 2, 2, 2, 2, 2, 2, 2, 2, 2, 2, 2, 2, 2, 2, 2, 2, 2, 2, 2, 2, 2, 2, 2, 2, 2, 2, 2, 2, 2, 2, 2, 2, 2, 2, 2, 3 ),
 ( 0.000000000000000000, 1.000000000000000000 ),
 ( 0.000000000000000000, 0.01388888888888888812, 0.02777777777777777624, 0.04166666666666666435, 0.05555555555555555247, 0.06944444444444444753, 0.08333333333333332871, 0.09722222222222222376, 0.1111111111111111049, 0.1250000000000000000, 0.1388888888888888951, 0.1527777777777777901, 0.1666666666666666574, 0.1805555555555555525, 0.1944444444444444475, 0.2083333333333333426, 0.2222222222222222099, 0.2361111111111111049, 0.2500000000000000000, 0.2638888888888888951, 0.2777777777777777901, 0.2916666666666666852, 0.3055555555555555802, 0.3194444444444444198, 0.3333333333333333148, 0.3472222222222222099, 0.3611111111111111049, 0.3750000000000000000, 0.3888888888888888951, 0.4027777777777777901, 0.4166666666666666852, 0.4305555555555555802, 0.4444444444444444198, 0.4583333333333333148, 0.4722222222222222099, 0.4861111111111111049, 0.5000000000000000000, 0.5138888888888888395, 0.5277777777777777901, 0.5416666666666666297, 0.5555555555555555802, 0.5694444444444444198, 0.5833333333333333703, 0.5972222222222222099, 0.6111111111111111605, 0.6250000000000000000, 0.6388888888888888395, 0.6527777777777777901, 0.6666666666666666297, 0.6805555555555555802, 0.6944444444444444198, 0.7083333333333333703, 0.7222222222222222099, 0.7361111111111111605, 0.7500000000000000000, 0.7638888888888888395, 0.7777777777777777901, 0.7916666666666666297, 0.8055555555555555802, 0.8194444444444444198, 0.8333333333333333703, 0.8472222222222222099, 0.8611111111111111605, 0.8750000000000000000, 0.8888888888888888395, 0.9027777777777777901, 0.9166666666666666297, 0.9258785565094813652 ),
 .UNSPECIFIED. ) 
 GEOMETRIC_REPRESENTATION_ITEM ( )  RATIONAL_B_SPLINE_SURFACE ( (
 ( 1.000000000000000000, 0.8660254037844387076, 1.000000000000000000, 0.8660254037844387076, 1.000000000000000000, 0.8660254037844387076, 1.000000000000000000, 0.8660254037844387076, 1.000000000000000000, 0.8660254037844387076, 1.000000000000000000, 0.8660254037844387076, 1.000000000000000000, 0.8660254037844387076, 1.000000000000000000, 0.8660254037844387076, 1.000000000000000000, 0.8660254037844387076, 1.000000000000000000, 0.8660254037844387076, 1.000000000000000000, 0.8660254037844387076, 1.000000000000000000, 0.8660254037844387076, 1.000000000000000000, 0.8660254037844387076, 1.000000000000000000, 0.8660254037844387076, 1.000000000000000000, 0.8660254037844387076, 1.000000000000000000, 0.8660254037844387076, 1.000000000000000000, 0.8660254037844387076, 1.000000000000000000, 0.8660254037844387076, 1.000000000000000000, 0.8660254037844387076, 1.000000000000000000, 0.8660254037844387076, 1.000000000000000000, 0.8660254037844387076, 1.000000000000000000, 0.8660254037844387076, 1.000000000000000000, 0.8660254037844387076, 1.000000000000000000, 0.8660254037844387076, 1.000000000000000000, 0.8660254037844387076, 1.000000000000000000, 0.8660254037844387076, 1.000000000000000000, 0.8660254037844387076, 1.000000000000000000, 0.8660254037844387076, 1.000000000000000000, 0.8660254037844387076, 1.000000000000000000, 0.8660254037844387076, 1.000000000000000000, 0.8660254037844387076, 1.000000000000000000, 0.8660254037844387076, 1.000000000000000000, 0.8660254037844387076, 1.000000000000000000, 0.8660254037844387076, 1.000000000000000000, 0.8660254037844387076, 1.000000000000000000, 0.8660254037844387076, 1.000000000000000000, 0.8660254037844387076, 1.000000000000000000, 0.8660254037844387076, 1.000000000000000000, 0.8660254037844387076, 1.000000000000000000, 0.8660254037844387076, 1.000000000000000000, 0.8660254037844387076, 1.000000000000000000, 0.8660254037844387076, 1.000000000000000000, 0.8660254037844387076, 1.000000000000000000, 0.8660254037844387076, 1.000000000000000000, 0.8660254037844387076, 1.000000000000000000, 0.8660254037844387076, 1.000000000000000000, 0.8660254037844387076, 1.000000000000000000, 0.8660254037844387076, 1.000000000000000000, 0.8660254037844387076, 1.000000000000000000, 0.8660254037844387076, 1.000000000000000000, 0.8660254037844387076, 1.000000000000000000, 0.8660254037844387076, 1.000000000000000000, 0.8660254037844387076, 1.000000000000000000, 0.8660254037844387076, 1.000000000000000000, 0.8660254037844387076, 1.000000000000000000, 0.8660254037844387076, 1.000000000000000000, 0.8660254037844387076, 1.000000000000000000, 0.8660254037844387076, 1.000000000000000000, 0.8660254037844387076, 1.000000000000000000, 0.8660254037844387076, 1.000000000000000000, 0.8660254037844387076, 1.000000000000000000, 0.8660254037844387076, 1.000000000000000000, 0.8660254037844387076, 1.000000000000000000, 0.8660254037844387076, 1.000000000000000000, 0.8660254037844387076, 1.000000000000000000, 0.8660254037844387076, 1.000000000000000000, 0.9111405360107203144, 0.9401542295229963209),
 ( 1.000000000000000000, 0.8660254037844387076, 1.000000000000000000, 0.8660254037844387076, 1.000000000000000000, 0.8660254037844387076, 1.000000000000000000, 0.8660254037844387076, 1.000000000000000000, 0.8660254037844387076, 1.000000000000000000, 0.8660254037844387076, 1.000000000000000000, 0.8660254037844387076, 1.000000000000000000, 0.8660254037844387076, 1.000000000000000000, 0.8660254037844387076, 1.000000000000000000, 0.8660254037844387076, 1.000000000000000000, 0.8660254037844387076, 1.000000000000000000, 0.8660254037844387076, 1.000000000000000000, 0.8660254037844387076, 1.000000000000000000, 0.8660254037844387076, 1.000000000000000000, 0.8660254037844387076, 1.000000000000000000, 0.8660254037844387076, 1.000000000000000000, 0.8660254037844387076, 1.000000000000000000, 0.8660254037844387076, 1.000000000000000000, 0.8660254037844387076, 1.000000000000000000, 0.8660254037844387076, 1.000000000000000000, 0.8660254037844387076, 1.000000000000000000, 0.8660254037844387076, 1.000000000000000000, 0.8660254037844387076, 1.000000000000000000, 0.8660254037844387076, 1.000000000000000000, 0.8660254037844387076, 1.000000000000000000, 0.8660254037844387076, 1.000000000000000000, 0.8660254037844387076, 1.000000000000000000, 0.8660254037844387076, 1.000000000000000000, 0.8660254037844387076, 1.000000000000000000, 0.8660254037844387076, 1.000000000000000000, 0.8660254037844387076, 1.000000000000000000, 0.8660254037844387076, 1.000000000000000000, 0.8660254037844387076, 1.000000000000000000, 0.8660254037844387076, 1.000000000000000000, 0.8660254037844387076, 1.000000000000000000, 0.8660254037844387076, 1.000000000000000000, 0.8660254037844387076, 1.000000000000000000, 0.8660254037844387076, 1.000000000000000000, 0.8660254037844387076, 1.000000000000000000, 0.8660254037844387076, 1.000000000000000000, 0.8660254037844387076, 1.000000000000000000, 0.8660254037844387076, 1.000000000000000000, 0.8660254037844387076, 1.000000000000000000, 0.8660254037844387076, 1.000000000000000000, 0.8660254037844387076, 1.000000000000000000, 0.8660254037844387076, 1.000000000000000000, 0.8660254037844387076, 1.000000000000000000, 0.8660254037844387076, 1.000000000000000000, 0.8660254037844387076, 1.000000000000000000, 0.8660254037844387076, 1.000000000000000000, 0.8660254037844387076, 1.000000000000000000, 0.8660254037844387076, 1.000000000000000000, 0.8660254037844387076, 1.000000000000000000, 0.8660254037844387076, 1.000000000000000000, 0.8660254037844387076, 1.000000000000000000, 0.8660254037844387076, 1.000000000000000000, 0.8660254037844387076, 1.000000000000000000, 0.8660254037844387076, 1.000000000000000000, 0.8660254037844387076, 1.000000000000000000, 0.8660254037844387076, 1.000000000000000000, 0.8660254037844387076, 1.000000000000000000, 0.8660254037844387076, 1.000000000000000000, 0.8660254037844387076, 1.000000000000000000, 0.8660254037844387076, 1.000000000000000000, 0.8660254037844387076, 1.000000000000000000, 0.8660254037844387076, 1.000000000000000000, 0.9111405360107203144, 0.9401542295229963209) ) ) 
 REPRESENTATION_ITEM ( '' )  SURFACE ( )  );
#17227 = AXIS2_PLACEMENT_3D ( 'NONE', #1103, #2760, #2558 ) ;
#17228 = DIRECTION ( 'NONE',  ( 0.000000000000000000, 1.000000000000000000, 0.000000000000000000 ) ) ;
#17229 = CARTESIAN_POINT ( 'NONE',  ( 231.2217848218749339, -33.32812499938548001, 102.3871387122750889 ) ) ;
#17230 = CARTESIAN_POINT ( 'NONE',  ( -85.15643035624999868, -33.81562499938549138, 101.5914258081833879 ) ) ;
#17231 = CARTESIAN_POINT ( 'NONE',  ( 232.5999999999999375, -30.70312499938548001, -53.18285161636690361 ) ) ;
#17232 = ORIENTED_EDGE ( 'NONE', *, *, #18460, .F. ) ;
#17233 = CARTESIAN_POINT ( 'NONE',  ( -80.80861089413674847, -34.99999999999999289, -97.72105564972109448 ) ) ;
#17234 = CARTESIAN_POINT ( 'NONE',  ( -81.02178482187500208, -34.49062499938548854, 102.3871387122750889 ) ) ;
#17235 = CARTESIAN_POINT ( 'NONE',  ( 79.77811200999867935, -34.99999999999999289, 99.14934632385235602 ) ) ;
#17236 = CARTESIAN_POINT ( 'NONE',  ( 82.39999999999999147, -32.50312499938548427, 103.1828516163667899 ) ) ;
#17237 = DIRECTION ( 'NONE',  ( -1.000000000000000000, -0.000000000000000000, -0.000000000000000000 ) ) ;
#17238 = EDGE_CURVE ( 'NONE', #9425, #2466, #8708, .T. ) ;
#17239 = AXIS2_PLACEMENT_3D ( 'NONE', #12019, #4603, #7434 ) ;
#17240 = EDGE_CURVE ( 'NONE', #10655, #10520, #11412, .T. ) ;
#17241 = LINE ( 'NONE', #8435, #2364 ) ;
#17242 = CARTESIAN_POINT ( 'NONE',  ( -79.64356964374999848, -34.07812499938548711, 99.99999999999998579 ) ) ;
#17243 = CARTESIAN_POINT ( 'NONE',  ( -83.77821517812500929, -34.22812499938549280, -97.61286128772489690 ) ) ;
#17244 = CARTESIAN_POINT ( 'NONE',  ( 81.02178482187500208, -31.79062499938548925, 97.61286128772489690 ) ) ;
#17245 = CARTESIAN_POINT ( 'NONE',  ( 85.15643035624999868, -33.81562499938549138, -101.5914258081833879 ) ) ;
#17246 = CARTESIAN_POINT ( 'NONE',  ( 235.3564303562499447, -32.61562499938548143, -50.00000000000011369 ) ) ;
#17247 = CARTESIAN_POINT ( 'NONE',  ( -81.02178482187500208, -33.59062499938548285, 102.3871387122750889 ) ) ;
#17248 = CARTESIAN_POINT ( 'NONE',  ( -96.99999999999998579, -5.200000000000000178, 150.0000000000000000 ) ) ;
#17249 = ADVANCED_FACE ( 'NONE', ( #16041 ), #1009, .F. ) ;
#17250 = VERTEX_POINT ( 'NONE', #322 ) ;
#17251 = CARTESIAN_POINT ( 'NONE',  ( 82.39999999999999147, -32.84062499938548996, 96.81714838363319586 ) ) ;
#17252 = CARTESIAN_POINT ( 'NONE',  ( 4.175648173966055587, -2.207990556236547608, -3.469390959564065291 ) ) ;
#17253 = CARTESIAN_POINT ( 'NONE',  ( -82.39999999999999147, -34.38750000000000284, 103.4641016151377499 ) ) ;
#17254 = AXIS2_PLACEMENT_3D ( 'NONE', #6745, #3318, #15333 ) ;
#17255 = CARTESIAN_POINT ( 'NONE',  ( -79.64356964375001269, -30.77812499938548285, 98.40857419181659793 ) ) ;
#17256 = AXIS2_PLACEMENT_3D ( 'NONE', #4736, #4534, #10682 ) ;
#17257 = CARTESIAN_POINT ( 'NONE',  ( -79.64356964375001269, -30.85312499938548569, 101.5914258081833879 ) ) ;
#17258 = CARTESIAN_POINT ( 'NONE',  ( 85.40000000000000568, -34.91250000000000142, 98.26794919243111792 ) ) ;
#17259 = ORIENTED_EDGE ( 'NONE', *, *, #11875, .T. ) ;
#17260 = CARTESIAN_POINT ( 'NONE',  ( -79.39999999999999147, -32.51250000000000284, -98.26794919243113213 ) ) ;
#17261 = FACE_OUTER_BOUND ( 'NONE', #7823, .T. ) ;
#17262 = CARTESIAN_POINT ( 'NONE',  ( 94.79999999999995453, -29.80000000000000071, 150.0000000000000000 ) ) ;
#17263 = CARTESIAN_POINT ( 'NONE',  ( 80.90000000000000568, -32.04374999877096997, -102.5980762113533018 ) ) ;
#17264 = CARTESIAN_POINT ( 'NONE',  ( 3.958484000407027636, 2.327740518749021437, -2.968235154689955024 ) ) ;
#17265 = CARTESIAN_POINT ( 'NONE',  ( -84.12112955302457351, -35.00000000000000000, 97.53419980903896658 ) ) ;
#17266 = DIRECTION ( 'NONE',  ( 0.000000000000000000, -1.000000000000000000, 0.000000000000000000 ) ) ;
#17267 = CARTESIAN_POINT ( 'NONE',  ( 82.05869624310412291, -34.96883842999723413, 97.01420019955246232 ) ) ;
#17268 = CARTESIAN_POINT ( 'NONE',  ( 82.39999999999999147, -31.26562499938549067, 103.1828516163667899 ) ) ;
#17269 = VECTOR ( 'NONE', #17502, 1000.000000000000000 ) ;
#17270 = CYLINDRICAL_SURFACE ( 'NONE', #18681, 3.000000000000009770 ) ;
#17271 = CLOSED_SHELL ( 'NONE', ( #15851, #9508, #12930, #9714, #10480, #14474, #10180, #12562, #18242, #4354, #255, #16184, #550, #15944, #5704, #14599, #17001 ) ) ;
#17272 = DIRECTION ( 'NONE',  ( 0.000000000000000000, -1.000000000000000000, 0.000000000000000000 ) ) ;
#17273 = CARTESIAN_POINT ( 'NONE',  ( 85.15643035624999868, -32.99062499938548854, -98.40857419181659793 ) ) ;
#17274 = CARTESIAN_POINT ( 'NONE',  ( 81.59615242270665192, -32.77634618820330559, 103.0000000000000000 ) ) ;
#17275 = ORIENTED_EDGE ( 'NONE', *, *, #9967, .F. ) ;
#17276 =( BOUNDED_SURFACE ( )  B_SPLINE_SURFACE ( 1, 2, ( 
 ( #6654, #5091, #699, #5183, #9675, #17098, #8686, #17677, #14348, #8582, #4291, #13268, #18861, #16218, #1073, #1170, #6940, #19241, #7312, #9968, #17581, #10060, #13173, #10256, #4096, #15922, #1270, #8779, #2823, #16018, #10154, #984, #5482, #2620, #14536, #11428, #4003, #7031, #7128, #14636, #14732, #1367, #7217, #10344, #13080, #12985, #17390, #5858, #2723, #14440, #5579, #16115, #11812, #17780, #18955, #19143, #19048, #2525, #11526, #4388, #5671, #11614, #8485, #5759, #4192, #16310, #11710, #12890, #2918, #17489, #4680, #4783, #7697, #1739, #13554, #16688, #5, #16595, #13464, #6052, #6341, #196, #15029, #18258, #11999, #3201, #18069, #3297, #9160, #12191, #8871, #3106, #18160, #7795, #13372, #10725, #14935, #1651, #1456, #13749, #1835, #4483, #12096, #4580, #13653, #9254, #17968, #10436, #15124, #15219, #387, #296, #14829, #1560, #5954, #7409, #12292, #11903, #17874, #4875, #10818, #16503, #16785, #16402, #10630, #10536, #3010, #8968, #6244, #7507, #102, #9064, #7603, #6145, #7985 ),
 ( #11105, #13941, #9745, #5065, #2129, #579, #6625, #18742, #768, #8088, #14226, #12773, #675, #12479, #3778, #15313, #3687, #3587, #12386, #9448, #17175, #14040, #18447, #482, #17073, #12575, #865, #11008, #1926, #9547, #3399, #18542, #18641, #2218, #15613, #5158, #11210, #13840, #9653, #6533, #16975, #6828, #8183, #15513, #5361, #14133, #6722, #12668, #15710, #5264, #2312, #9350, #8276, #11304, #7890, #6434, #18353, #15413, #4976, #10917, #16884, #3487, #2023, #1146, #12961, #16090, #1243, #7007, #18839, #4172, #11686, #19118, #5646, #17273, #9940, #8373, #9840, #8753, #14326, #964, #16193, #14705, #5553, #5737, #7289, #7104, #14416, #7195, #17654, #8655, #2801, #13059, #8462, #13144, #1342, #2505, #19025, #18932, #1053, #6919, #11592, #11500, #4266, #17464, #15993, #4075, #17558, #13244, #14613, #2598, #19216, #5833, #14510, #10035, #10227, #15805, #10132, #8558, #2696, #3878, #2410, #12867, #5461, #11403, #17365, #3975, #15898, #11974, #6120, #1715, #7669, #12072, #7772, #17942, #17846 ) ),
 .UNSPECIFIED., .F., .F., .F. ) 
 B_SPLINE_SURFACE_WITH_KNOTS ( ( 2, 2 ),
 ( 3, 2, 2, 2, 2, 2, 2, 2, 2, 2, 2, 2, 2, 2, 2, 2, 2, 2, 2, 2, 2, 2, 2, 2, 2, 2, 2, 2, 2, 2, 2, 2, 2, 2, 2, 2, 2, 2, 2, 2, 2, 2, 2, 2, 2, 2, 2, 2, 2, 2, 2, 2, 2, 2, 2, 2, 2, 2, 2, 2, 2, 2, 2, 2, 2, 2, 2, 3 ),
 ( 0.000000000000000000, 1.000000000000000000 ),
 ( 0.000000000000000000, 0.01388888888888888812, 0.02777777777777777624, 0.04166666666666666435, 0.05555555555555555247, 0.06944444444444444753, 0.08333333333333332871, 0.09722222222222222376, 0.1111111111111111049, 0.1250000000000000000, 0.1388888888888888951, 0.1527777777777777901, 0.1666666666666666574, 0.1805555555555555525, 0.1944444444444444475, 0.2083333333333333426, 0.2222222222222222099, 0.2361111111111111049, 0.2500000000000000000, 0.2638888888888888951, 0.2777777777777777901, 0.2916666666666666852, 0.3055555555555555802, 0.3194444444444444198, 0.3333333333333333148, 0.3472222222222222099, 0.3611111111111111049, 0.3750000000000000000, 0.3888888888888888951, 0.4027777777777777901, 0.4166666666666666852, 0.4305555555555555802, 0.4444444444444444198, 0.4583333333333333148, 0.4722222222222222099, 0.4861111111111111049, 0.5000000000000000000, 0.5138888888888888395, 0.5277777777777777901, 0.5416666666666666297, 0.5555555555555555802, 0.5694444444444444198, 0.5833333333333333703, 0.5972222222222222099, 0.6111111111111111605, 0.6250000000000000000, 0.6388888888888888395, 0.6527777777777777901, 0.6666666666666666297, 0.6805555555555555802, 0.6944444444444444198, 0.7083333333333333703, 0.7222222222222222099, 0.7361111111111111605, 0.7500000000000000000, 0.7638888888888888395, 0.7777777777777777901, 0.7916666666666666297, 0.8055555555555555802, 0.8194444444444444198, 0.8333333333333333703, 0.8472222222222222099, 0.8611111111111111605, 0.8750000000000000000, 0.8888888888888888395, 0.9027777777777777901, 0.9166666666666666297, 0.9258785144422092550 ),
 .UNSPECIFIED. ) 
 GEOMETRIC_REPRESENTATION_ITEM ( )  RATIONAL_B_SPLINE_SURFACE ( (
 ( 1.000000000000000000, 0.8660254037844387076, 1.000000000000000000, 0.8660254037844387076, 1.000000000000000000, 0.8660254037844387076, 1.000000000000000000, 0.8660254037844387076, 1.000000000000000000, 0.8660254037844387076, 1.000000000000000000, 0.8660254037844387076, 1.000000000000000000, 0.8660254037844387076, 1.000000000000000000, 0.8660254037844387076, 1.000000000000000000, 0.8660254037844387076, 1.000000000000000000, 0.8660254037844387076, 1.000000000000000000, 0.8660254037844387076, 1.000000000000000000, 0.8660254037844387076, 1.000000000000000000, 0.8660254037844387076, 1.000000000000000000, 0.8660254037844387076, 1.000000000000000000, 0.8660254037844387076, 1.000000000000000000, 0.8660254037844387076, 1.000000000000000000, 0.8660254037844387076, 1.000000000000000000, 0.8660254037844387076, 1.000000000000000000, 0.8660254037844387076, 1.000000000000000000, 0.8660254037844387076, 1.000000000000000000, 0.8660254037844387076, 1.000000000000000000, 0.8660254037844387076, 1.000000000000000000, 0.8660254037844387076, 1.000000000000000000, 0.8660254037844387076, 1.000000000000000000, 0.8660254037844387076, 1.000000000000000000, 0.8660254037844387076, 1.000000000000000000, 0.8660254037844387076, 1.000000000000000000, 0.8660254037844387076, 1.000000000000000000, 0.8660254037844387076, 1.000000000000000000, 0.8660254037844387076, 1.000000000000000000, 0.8660254037844387076, 1.000000000000000000, 0.8660254037844387076, 1.000000000000000000, 0.8660254037844387076, 1.000000000000000000, 0.8660254037844387076, 1.000000000000000000, 0.8660254037844387076, 1.000000000000000000, 0.8660254037844387076, 1.000000000000000000, 0.8660254037844387076, 1.000000000000000000, 0.8660254037844387076, 1.000000000000000000, 0.8660254037844387076, 1.000000000000000000, 0.8660254037844387076, 1.000000000000000000, 0.8660254037844387076, 1.000000000000000000, 0.8660254037844387076, 1.000000000000000000, 0.8660254037844387076, 1.000000000000000000, 0.8660254037844387076, 1.000000000000000000, 0.8660254037844387076, 1.000000000000000000, 0.8660254037844387076, 1.000000000000000000, 0.8660254037844387076, 1.000000000000000000, 0.8660254037844387076, 1.000000000000000000, 0.8660254037844387076, 1.000000000000000000, 0.8660254037844387076, 1.000000000000000000, 0.8660254037844387076, 1.000000000000000000, 0.8660254037844387076, 1.000000000000000000, 0.8660254037844387076, 1.000000000000000000, 0.8660254037844387076, 1.000000000000000000, 0.8660254037844387076, 1.000000000000000000, 0.8660254037844387076, 1.000000000000000000, 0.8660254037844387076, 1.000000000000000000, 0.8660254037844387076, 1.000000000000000000, 0.8660254037844387076, 1.000000000000000000, 0.8660254037844387076, 1.000000000000000000, 0.8660254037844387076, 1.000000000000000000, 0.8660254037844387076, 1.000000000000000000, 0.8660254037844387076, 1.000000000000000000, 0.8660254037844387076, 1.000000000000000000, 0.8660254037844387076, 1.000000000000000000, 0.8660254037844387076, 1.000000000000000000, 0.9111409417988175496, 0.9401539645359766606),
 ( 1.000000000000000000, 0.8660254037844387076, 1.000000000000000000, 0.8660254037844387076, 1.000000000000000000, 0.8660254037844387076, 1.000000000000000000, 0.8660254037844387076, 1.000000000000000000, 0.8660254037844387076, 1.000000000000000000, 0.8660254037844387076, 1.000000000000000000, 0.8660254037844387076, 1.000000000000000000, 0.8660254037844387076, 1.000000000000000000, 0.8660254037844387076, 1.000000000000000000, 0.8660254037844387076, 1.000000000000000000, 0.8660254037844387076, 1.000000000000000000, 0.8660254037844387076, 1.000000000000000000, 0.8660254037844387076, 1.000000000000000000, 0.8660254037844387076, 1.000000000000000000, 0.8660254037844387076, 1.000000000000000000, 0.8660254037844387076, 1.000000000000000000, 0.8660254037844387076, 1.000000000000000000, 0.8660254037844387076, 1.000000000000000000, 0.8660254037844387076, 1.000000000000000000, 0.8660254037844387076, 1.000000000000000000, 0.8660254037844387076, 1.000000000000000000, 0.8660254037844387076, 1.000000000000000000, 0.8660254037844387076, 1.000000000000000000, 0.8660254037844387076, 1.000000000000000000, 0.8660254037844387076, 1.000000000000000000, 0.8660254037844387076, 1.000000000000000000, 0.8660254037844387076, 1.000000000000000000, 0.8660254037844387076, 1.000000000000000000, 0.8660254037844387076, 1.000000000000000000, 0.8660254037844387076, 1.000000000000000000, 0.8660254037844387076, 1.000000000000000000, 0.8660254037844387076, 1.000000000000000000, 0.8660254037844387076, 1.000000000000000000, 0.8660254037844387076, 1.000000000000000000, 0.8660254037844387076, 1.000000000000000000, 0.8660254037844387076, 1.000000000000000000, 0.8660254037844387076, 1.000000000000000000, 0.8660254037844387076, 1.000000000000000000, 0.8660254037844387076, 1.000000000000000000, 0.8660254037844387076, 1.000000000000000000, 0.8660254037844387076, 1.000000000000000000, 0.8660254037844387076, 1.000000000000000000, 0.8660254037844387076, 1.000000000000000000, 0.8660254037844387076, 1.000000000000000000, 0.8660254037844387076, 1.000000000000000000, 0.8660254037844387076, 1.000000000000000000, 0.8660254037844387076, 1.000000000000000000, 0.8660254037844387076, 1.000000000000000000, 0.8660254037844387076, 1.000000000000000000, 0.8660254037844387076, 1.000000000000000000, 0.8660254037844387076, 1.000000000000000000, 0.8660254037844387076, 1.000000000000000000, 0.8660254037844387076, 1.000000000000000000, 0.8660254037844387076, 1.000000000000000000, 0.8660254037844387076, 1.000000000000000000, 0.8660254037844387076, 1.000000000000000000, 0.8660254037844387076, 1.000000000000000000, 0.8660254037844387076, 1.000000000000000000, 0.8660254037844387076, 1.000000000000000000, 0.8660254037844387076, 1.000000000000000000, 0.8660254037844387076, 1.000000000000000000, 0.8660254037844387076, 1.000000000000000000, 0.8660254037844387076, 1.000000000000000000, 0.8660254037844387076, 1.000000000000000000, 0.8660254037844387076, 1.000000000000000000, 0.8660254037844387076, 1.000000000000000000, 0.9111409417988175496, 0.9401539645359766606) ) ) 
 REPRESENTATION_ITEM ( '' )  SURFACE ( )  );
#17277 = CARTESIAN_POINT ( 'NONE',  ( 85.40000000000000568, -31.29374999877096997, 99.99999999999998579 ) ) ;
#17278 = CARTESIAN_POINT ( 'NONE',  ( 229.8435696437499871, -35.16562499938547148, 101.5914258081833879 ) ) ;
#17279 = CARTESIAN_POINT ( 'NONE',  ( 229.8435696437499871, -34.26562499938548001, -48.40857419181671162 ) ) ;
#17280 = CARTESIAN_POINT ( 'NONE',  ( 85.40000000000000568, -34.50000000000000000, 99.99999999999998579 ) ) ;
#17281 = CARTESIAN_POINT ( 'NONE',  ( 109.9999999999999432, -29.80000000000002558, -150.0000000000000000 ) ) ;
#17282 = ORIENTED_EDGE ( 'NONE', *, *, #10313, .F. ) ;
#17283 = EDGE_CURVE ( 'NONE', #18266, #14464, #3237, .T. ) ;
#17284 = CARTESIAN_POINT ( 'NONE',  ( -85.15643035624999868, -32.35312499938549280, -98.40857419181659793 ) ) ;
#17285 = CARTESIAN_POINT ( 'NONE',  ( 85.40000000000000568, -33.11250000000000426, 98.26794919243111792 ) ) ;
#17286 = EDGE_LOOP ( 'NONE', ( #3735, #7424, #6157, #38 ) ) ;
#17287 = CARTESIAN_POINT ( 'NONE',  ( 82.39999999999999147, -32.39062499938548711, 96.81714838363319586 ) ) ;
#17288 = CARTESIAN_POINT ( 'NONE',  ( -83.77821517812500929, -30.62812499938548783, -97.61286128772489690 ) ) ;
#17289 = CARTESIAN_POINT ( 'NONE',  ( 85.40000000000000568, -34.05000000000000426, 99.99999999999998579 ) ) ;
#17290 = DIRECTION ( 'NONE',  ( -1.000000000000000000, -0.000000000000000000, -0.000000000000000000 ) ) ;
#17291 = CARTESIAN_POINT ( 'NONE',  ( -83.90000000000000568, -34.36874999877097281, 102.5980762113533018 ) ) ;
#17292 = CARTESIAN_POINT ( 'NONE',  ( -85.15643035625001289, -32.05312499938548854, 99.99999999999998579 ) ) ;
#17293 = CARTESIAN_POINT ( 'NONE',  ( -79.64356964374998427, -32.12812499938548427, -101.5914258081833879 ) ) ;
#17294 = CARTESIAN_POINT ( 'NONE',  ( -82.40000000000000568, -34.10624999877096997, -102.9999999999999858 ) ) ;
#17295 = LINE ( 'NONE', #3709, #4781 ) ;
#17296 = CARTESIAN_POINT ( 'NONE',  ( 235.5999999999999943, -30.71249999999999858, 101.7320508075688537 ) ) ;
#17297 = EDGE_LOOP ( 'NONE', ( #2527, #18476, #15925, #9458 ) ) ;
#17298 = CARTESIAN_POINT ( 'NONE',  ( 79.64356964374999848, -33.51562499938548711, -99.99999999999998579 ) ) ;
#17299 = CARTESIAN_POINT ( 'NONE',  ( 229.5999999999999375, -33.99374999877096570, 99.99999999999998579 ) ) ;
#17300 = CARTESIAN_POINT ( 'NONE',  ( 231.0999999999999375, -32.26874999877096428, -52.59807621135342970 ) ) ;
#17301 = EDGE_LOOP ( 'NONE', ( #16598, #3210, #9484 ) ) ;
#17302 = CARTESIAN_POINT ( 'NONE',  ( 85.40000000000000568, -32.66250000000000142, 98.26794919243111792 ) ) ;
#17303 = CARTESIAN_POINT ( 'NONE',  ( -81.02178482187500208, -31.64062499938548356, 97.61286128772489690 ) ) ;
#17304 = CARTESIAN_POINT ( 'NONE',  ( 3.806834918298646731, 3.031088913245537864, 1.750000000000000666 ) ) ;
#17305 = ORIENTED_EDGE ( 'NONE', *, *, #17735, .F. ) ;
#17306 = CARTESIAN_POINT ( 'NONE',  ( -83.20384757729335945, -34.08615380933863293, -102.9999999999999858 ) ) ;
#17307 = CARTESIAN_POINT ( 'NONE',  ( 232.5999999999999375, -33.20624999877097139, 97.00000000000000000 ) ) ;
#17308 = VERTEX_POINT ( 'NONE', #5977 ) ;
#17309 =( BOUNDED_CURVE ( )  B_SPLINE_CURVE ( 2, ( #3171, #10409, #10604, #9222, #68, #4359, #10696, #6116, #1804 ),
 .UNSPECIFIED., .F., .F. ) 
 B_SPLINE_CURVE_WITH_KNOTS ( ( 3, 2, 2, 2, 3 ),
 ( 0.4375000000000000555, 0.4444444444444444198, 0.4583333333333333148, 0.4722222222222222099, 0.4791666666666666297 ),
 .UNSPECIFIED. ) 
 CURVE ( )  GEOMETRIC_REPRESENTATION_ITEM ( )  RATIONAL_B_SPLINE_CURVE ( ( 0.9330127018922192983, 0.9330127018922198534, 1.000000000000000000, 0.8660254037844387076, 1.000000000000000000, 0.8660254037844387076, 1.000000000000000000, 0.9330127018922196314, 0.9330127018922194093 ) ) 
 REPRESENTATION_ITEM ( '' )  );
#17310 = DIRECTION ( 'NONE',  ( -1.000000000000000000, -0.000000000000000000, 0.000000000000000000 ) ) ;
#17311 = CARTESIAN_POINT ( 'NONE',  ( 79.39999999999999147, -33.78750000000000142, -98.26794919243110371 ) ) ;
#17312 = CARTESIAN_POINT ( 'NONE',  ( 0.1397371499203167999, 1.362866705341264417, 3.499999999999999556 ) ) ;
#17313 = CARTESIAN_POINT ( 'NONE',  ( -83.77821517812500929, -31.22812499938548569, 97.61286128772489690 ) ) ;
#17314 = CARTESIAN_POINT ( 'NONE',  ( -83.90000000000000568, -34.87106250001230023, 102.5980762113533018 ) ) ;
#17315 = CARTESIAN_POINT ( 'NONE',  ( 235.3594282536527089, -35.00000000000000000, -49.60353574117735320 ) ) ;
#17316 = SURFACE_SIDE_STYLE ('',( #4314 ) ) ;
#17317 = CARTESIAN_POINT ( 'NONE',  ( 84.05108659120818970, -32.00820041275124339, 102.2295963284773563 ) ) ;
#17318 = CARTESIAN_POINT ( 'NONE',  ( 81.59615242270662350, -33.91740381056766296, 96.99999999999997158 ) ) ;
#17319 = CARTESIAN_POINT ( 'NONE',  ( 83.43443729601550274, -34.99999999999999289, 97.42249611015769517 ) ) ;
#17320 = CARTESIAN_POINT ( 'NONE',  ( -4.000000000000000000, -2.309401076758512694, -5.000000000000000000 ) ) ;
#17321 = EDGE_LOOP ( 'NONE', ( #655, #8225, #620, #11723 ) ) ;
#17322 = CARTESIAN_POINT ( 'NONE',  ( 234.0999999999999375, -34.19999999999999574, -52.59807621135342970 ) ) ;
#17323 = CARTESIAN_POINT ( 'NONE',  ( 235.2646886264966213, -35.00000000000002132, 98.99456257074425025 ) ) ;
#17324 = FACE_OUTER_BOUND ( 'NONE', #15712, .T. ) ;
#17325 = CARTESIAN_POINT ( 'NONE',  ( 229.8435696437499587, -34.79062499938547859, 98.40857419181659793 ) ) ;
#17326 = CARTESIAN_POINT ( 'NONE',  ( -83.77821517812500929, -34.37812499938548427, 97.61286128772489690 ) ) ;
#17327 = CARTESIAN_POINT ( 'NONE',  ( 233.9782151781249411, -30.29062499938547859, -52.38713871227520968 ) ) ;
#17328 = ORIENTED_EDGE ( 'NONE', *, *, #178, .F. ) ;
#17329 = DIRECTION ( 'NONE',  ( 0.000000000000000000, 0.000000000000000000, 1.000000000000000000 ) ) ;
#17330 = CARTESIAN_POINT ( 'NONE',  ( -85.15643035624999868, -32.87812499938549138, 98.40857419181659793 ) ) ;
#17331 = EDGE_CURVE ( 'NONE', #5897, #1970, #14914, .T. ) ;
#17332 = CARTESIAN_POINT ( 'NONE',  ( 84.28136653320183314, -32.00000000000000711, 102.0145392219077394 ) ) ;
#17333 = CARTESIAN_POINT ( 'NONE',  ( 82.39999999999999147, -30.11250000000000426, 103.4641016151377499 ) ) ;
#17334 = CARTESIAN_POINT ( 'NONE',  ( 231.7961524227065979, -33.18615380933862724, -53.00000000000009948 ) ) ;
#17335 = AXIS2_PLACEMENT_3D ( 'NONE', #12907, #15936, #15651 ) ;
#17336 = CARTESIAN_POINT ( 'NONE',  ( 235.3564303562499447, -32.61562499938548143, -50.00000000000011369 ) ) ;
#17337 = CARTESIAN_POINT ( 'NONE',  ( -82.39999999999999147, -33.96562499938548285, 96.81714838363319586 ) ) ;
#17338 = CARTESIAN_POINT ( 'NONE',  ( -81.02178482187500208, -34.60312499938549280, -97.61286128772489690 ) ) ;
#17339 = CARTESIAN_POINT ( 'NONE',  ( 85.15643035624999868, -31.07812499938548356, 101.5914258081833879 ) ) ;
#17340 =( BOUNDED_CURVE ( )  B_SPLINE_CURVE ( 2, ( #15462, #3539, #17217, #436, #15752, #6381, #5207, #8029, #6477 ),
 .UNSPECIFIED., .F., .F. ) 
 B_SPLINE_CURVE_WITH_KNOTS ( ( 3, 2, 2, 2, 3 ),
 ( 0.3125000000000001665, 0.3194444444444444198, 0.3333333333333333148, 0.3472222222222222099, 0.3541666666666666297 ),
 .UNSPECIFIED. ) 
 CURVE ( )  GEOMETRIC_REPRESENTATION_ITEM ( )  RATIONAL_B_SPLINE_CURVE ( ( 0.9330127018922194093, 0.9330127018922209636, 1.000000000000000000, 0.8660254037844387076, 1.000000000000000000, 0.8660254037844387076, 1.000000000000000000, 0.9330127018922196314, 0.9330127018922194093 ) ) 
 REPRESENTATION_ITEM ( '' )  );
#17341 = CARTESIAN_POINT ( 'NONE',  ( 82.39999999999999147, -34.86562499938548854, -96.81714838363319586 ) ) ;
#17342 = CARTESIAN_POINT ( 'NONE',  ( 229.8435696437499871, -31.97812499938548214, -51.59142580818350865 ) ) ;
#17343 = CARTESIAN_POINT ( 'NONE',  ( -79.64356964374998427, -34.37812499938548427, 98.40857419181659793 ) ) ;
#17344 = CARTESIAN_POINT ( 'NONE',  ( 79.64356964375001269, -31.30312499938548854, -101.5914258081833879 ) ) ;
#17345 = ORIENTED_EDGE ( 'NONE', *, *, #13150, .T. ) ;
#17346 = CARTESIAN_POINT ( 'NONE',  ( -82.40000000000000568, -30.00000000000000355, -96.99999999999998579 ) ) ;
#17347 = CARTESIAN_POINT ( 'NONE',  ( 233.4038475772933339, -34.31115380933863435, -47.00000000000012790 ) ) ;
#17348 = CARTESIAN_POINT ( 'NONE',  ( -85.40000000000000568, -33.14999999999999858, 99.99999999999998579 ) ) ;
#17349 = CARTESIAN_POINT ( 'NONE',  ( -79.64356964374999848, -33.96562499938548285, 99.99999999999998579 ) ) ;
#17350 = CARTESIAN_POINT ( 'NONE',  ( -83.77821517812500929, -31.11562499938548498, 97.61286128772489690 ) ) ;
#17351 = CARTESIAN_POINT ( 'NONE',  ( 25.15499999999999758, 0.000000000000000000, 0.000000000000000000 ) ) ;
#17352 = CARTESIAN_POINT ( 'NONE',  ( -83.33080762004576059, -35.05289549976084373, -103.5578907812544855 ) ) ;
#17353 = CARTESIAN_POINT ( 'NONE',  ( 232.5999999999999943, -33.17812499938548143, 103.1828516163667899 ) ) ;
#17354 = CARTESIAN_POINT ( 'NONE',  ( 232.5999999999999375, -33.93749999999999289, -47.00000000000011369 ) ) ;
#17355 = CARTESIAN_POINT ( 'NONE',  ( -79.39999999999999147, -31.15856250001229455, 101.7320508075688537 ) ) ;
#17356 = MECHANICAL_DESIGN_GEOMETRIC_PRESENTATION_REPRESENTATION (  '', ( #14853 ), #14218 ) ;
#17357 = EDGE_CURVE ( 'NONE', #9562, #14525, #6747, .T. ) ;
#17358 = CARTESIAN_POINT ( 'NONE',  ( 4.055492966679589806, 3.795017426214568168, -0.5629142681441285934 ) ) ;
#17359 = CARTESIAN_POINT ( 'NONE',  ( 232.5999999999999375, -29.99999999999999645, 96.99999999999998579 ) ) ;
#17360 = CARTESIAN_POINT ( 'NONE',  ( -85.15643035624999868, -30.55312499938548854, 101.5914258081833879 ) ) ;
#17361 = LINE ( 'NONE', #3971, #4955 ) ;
#17362 = AXIS2_PLACEMENT_3D ( 'NONE', #11918, #17891, #13284 ) ;
#17363 = CARTESIAN_POINT ( 'NONE',  ( 234.3965303555544608, -32.00000000000000711, 97.67482724152034734 ) ) ;
#17364 = LINE ( 'NONE', #3974, #2147 ) ;
#17365 = CARTESIAN_POINT ( 'NONE',  ( 81.02178482187500208, -34.90312499938548285, -97.61286128772489690 ) ) ;
#17366 = CARTESIAN_POINT ( 'NONE',  ( 229.5999999999999375, -34.01249999999999574, 101.7320508075688821 ) ) ;
#17367 = ORIENTED_EDGE ( 'NONE', *, *, #6608, .F. ) ;
#17368 = CARTESIAN_POINT ( 'NONE',  ( 82.39999999999999147, -32.30624999877097281, 103.4641016151377499 ) ) ;
#17369 = CARTESIAN_POINT ( 'NONE',  ( 235.3564303562499447, -34.04062499938547859, 98.40857419181659793 ) ) ;
#17370 = CARTESIAN_POINT ( 'NONE',  ( 233.9782151781249411, -31.90312499938548285, -47.61286128772501769 ) ) ;
#17371 = EDGE_CURVE ( 'NONE', #14052, #5719, #14285, .T. ) ;
#17372 = CARTESIAN_POINT ( 'NONE',  ( -83.77821517812500929, -34.71562499938548285, 97.61286128772489690 ) ) ;
#17373 = DIRECTION ( 'NONE',  ( 0.000000000000000000, 0.000000000000000000, -1.000000000000000000 ) ) ;
#17374 = ORIENTED_EDGE ( 'NONE', *, *, #8667, .T. ) ;
#17375 = CARTESIAN_POINT ( 'NONE',  ( -85.15643035624999868, -31.97812499938548925, -101.5914258081833879 ) ) ;
#17376 = EDGE_CURVE ( 'NONE', #2879, #13090, #12023, .T. ) ;
#17377 = FACE_OUTER_BOUND ( 'NONE', #14772, .T. ) ;
#17378 = VERTEX_POINT ( 'NONE', #4506 ) ;
#17379 = CARTESIAN_POINT ( 'NONE',  ( 85.15643035625001289, -32.91562499938548569, 98.40857419181659793 ) ) ;
#17380 = CARTESIAN_POINT ( 'NONE',  ( -85.15643035625001289, -31.60312499938548569, -99.99999999999998579 ) ) ;
#17381 = CARTESIAN_POINT ( 'NONE',  ( 85.40000000000000568, -34.46249999999999858, 98.26794919243111792 ) ) ;
#17382 = CARTESIAN_POINT ( 'NONE',  ( 110.0000000000000142, 15.19999999999997797, -145.0000000000000000 ) ) ;
#17383 = CARTESIAN_POINT ( 'NONE',  ( -80.90000000000000568, -33.84374999877096712, 102.5980762113533018 ) ) ;
#17384 = PRESENTATION_LAYER_ASSIGNMENT (  '', '', ( #17704 ) ) ;
#17385 = CARTESIAN_POINT ( 'NONE',  ( -83.77821517812500929, -31.67812499938548498, 97.61286128772489690 ) ) ;
#17386 = CARTESIAN_POINT ( 'NONE',  ( -79.64356964374999848, -33.51562499938548711, -99.99999999999998579 ) ) ;
#17387 =( BOUNDED_CURVE ( )  B_SPLINE_CURVE ( 2, ( #14189, #12532, #1889, #12629, #8040, #3549, #6685, #16845, #10968 ),
 .UNSPECIFIED., .F., .F. ) 
 B_SPLINE_CURVE_WITH_KNOTS ( ( 3, 2, 2, 2, 3 ),
 ( 0.6458333333333333703, 0.6527777777777777901, 0.6666666666666666297, 0.6805555555555555802, 0.6875000000000000000 ),
 .UNSPECIFIED. ) 
 CURVE ( )  GEOMETRIC_REPRESENTATION_ITEM ( )  RATIONAL_B_SPLINE_CURVE ( ( 0.9330127018922192983, 0.9330127018922198534, 1.000000000000000000, 0.8660254037844387076, 1.000000000000000000, 0.8660254037844387076, 1.000000000000000000, 0.9330127018922194093, 0.9330127018922194093 ) ) 
 REPRESENTATION_ITEM ( '' )  );
#17388 = CARTESIAN_POINT ( 'NONE',  ( 230.5724978686189672, -35.00000000000000711, 97.77995849557630947 ) ) ;
#17389 = EDGE_CURVE ( 'NONE', #17445, #16126, #18665, .T. ) ;
#17390 = CARTESIAN_POINT ( 'NONE',  ( 83.90000000000000568, -32.11874999877097281, -102.5980762113533018 ) ) ;
#17391 = VECTOR ( 'NONE', #15803, 1000.000000000000000 ) ;
#17392 = CARTESIAN_POINT ( 'NONE',  ( 235.5999999999999375, -31.57499999999999218, 99.99999999999998579 ) ) ;
#17393 = ORIENTED_EDGE ( 'NONE', *, *, #7314, .F. ) ;
#17394 = CARTESIAN_POINT ( 'NONE',  ( 79.64356964374999848, -32.61562499938548854, -99.99999999999998579 ) ) ;
#17395 = CARTESIAN_POINT ( 'NONE',  ( 229.5999999999999375, -32.19374999877096144, 99.99999999999998579 ) ) ;
#17396 = CARTESIAN_POINT ( 'NONE',  ( 234.0999999999999375, -30.69374999877096499, -47.40192378864679768 ) ) ;
#17397 =( BOUNDED_CURVE ( )  B_SPLINE_CURVE ( 2, ( #18300, #3443, #6774, #5115, #9396, #8132, #10960, #12722, #4919 ),
 .UNSPECIFIED., .F., .F. ) 
 B_SPLINE_CURVE_WITH_KNOTS ( ( 3, 2, 2, 2, 3 ),
 ( 0.5208333333333334814, 0.5277777777777777901, 0.5416666666666666297, 0.5555555555555555802, 0.5625000000000000000 ),
 .UNSPECIFIED. ) 
 CURVE ( )  GEOMETRIC_REPRESENTATION_ITEM ( )  RATIONAL_B_SPLINE_CURVE ( ( 0.9330127018922194093, 0.9330127018922209636, 1.000000000000000000, 0.8660254037844387076, 1.000000000000000000, 0.8660254037844387076, 1.000000000000000000, 0.9330127018922194093, 0.9330127018922194093 ) ) 
 REPRESENTATION_ITEM ( '' )  );
#17398 = CARTESIAN_POINT ( 'NONE',  ( -79.39999999999999147, -35.08124999877097139, 98.26794919243110371 ) ) ;
#17399 = CARTESIAN_POINT ( 'NONE',  ( -79.64356964374998427, -30.40312499938548285, 101.5914258081833879 ) ) ;
#17400 = AXIS2_PLACEMENT_3D ( 'NONE', #7135, #16024, #2247 ) ;
#17401 = VERTEX_POINT ( 'NONE', #3036 ) ;
#17402 = ORIENTED_EDGE ( 'NONE', *, *, #12826, .T. ) ;
#17403 = CARTESIAN_POINT ( 'NONE',  ( 4.180231891692623769, -4.134807952925581453, -0.02076457676760805685 ) ) ;
#17404 = CARTESIAN_POINT ( 'NONE',  ( 4.082498951862918446, -2.020725942163687172, 3.500000000000002220 ) ) ;
#17405 = ORIENTED_EDGE ( 'NONE', *, *, #5561, .T. ) ;
#17406 = CARTESIAN_POINT ( 'NONE',  ( 105.1999999999999744, -29.80000000000002203, 150.0000000000000000 ) ) ;
#17407 = CARTESIAN_POINT ( 'NONE',  ( 83.90000000000000568, -32.62500000000000000, -102.5980762113533018 ) ) ;
#17408 = EDGE_CURVE ( 'NONE', #12671, #18799, #1765, .T. ) ;
#17409 = CARTESIAN_POINT ( 'NONE',  ( 79.79666399293472523, -31.99999999999998579, -101.4892189721552427 ) ) ;
#17410 = VECTOR ( 'NONE', #15757, 1000.000000000000000 ) ;
#17411 = CARTESIAN_POINT ( 'NONE',  ( -82.39999999999999147, -31.49062499938548854, 103.1828516163667899 ) ) ;
#17412 = CARTESIAN_POINT ( 'NONE',  ( -79.39999999999999147, -31.16250000000000497, 101.7320508075688537 ) ) ;
#17413 = CARTESIAN_POINT ( 'NONE',  ( 4.197393957002303999, 0.8151795401431359833, -3.503767560748935139 ) ) ;
#17414 = DIRECTION ( 'NONE',  ( 1.000000000000000000, 0.000000000000000000, 0.000000000000000000 ) ) ;
#17415 = CARTESIAN_POINT ( 'NONE',  ( 81.02178482187500208, -32.09062499938548285, 102.3871387122750889 ) ) ;
#17416 = CONICAL_SURFACE ( 'NONE', #4315, 3.500000000000000000, 1.047197551196600296 ) ;
#17417 = EDGE_CURVE ( 'NONE', #13089, #10928, #13337, .T. ) ;
#17418 = CARTESIAN_POINT ( 'NONE',  ( 79.77811200999867935, -34.99999999999999289, 99.14934632385235602 ) ) ;
#17419 = CARTESIAN_POINT ( 'NONE',  ( -82.39999999999999147, -34.52812499938548996, 103.1828516163667899 ) ) ;
#17420 = CARTESIAN_POINT ( 'NONE',  ( 85.15643035625001289, -35.09062499938548285, -99.99999999999998579 ) ) ;
#17421 = ORIENTED_EDGE ( 'NONE', *, *, #9884, .F. ) ;
#17422 = CARTESIAN_POINT ( 'NONE',  ( 81.59615242270662350, -33.01740381056767148, 96.99999999999998579 ) ) ;
#17423 = CIRCLE ( 'NONE', #13979, 2.649999999999985700 ) ;
#17424 = VECTOR ( 'NONE', #1600, 1000.000000000000000 ) ;
#17425 =( BOUNDED_CURVE ( )  B_SPLINE_CURVE ( 2, ( #1777, #6472, #15555, #3238, #9589, #16923, #12330, #4821, #10761 ),
 .UNSPECIFIED., .F., .F. ) 
 B_SPLINE_CURVE_WITH_KNOTS ( ( 3, 2, 2, 2, 3 ),
 ( 0.5208333333333334814, 0.5277777777777777901, 0.5416666666666666297, 0.5555555555555555802, 0.5625000000000000000 ),
 .UNSPECIFIED. ) 
 CURVE ( )  GEOMETRIC_REPRESENTATION_ITEM ( )  RATIONAL_B_SPLINE_CURVE ( ( 0.9330127018922194093, 0.9330127018922209636, 1.000000000000000000, 0.8660254037844387076, 1.000000000000000000, 0.8660254037844387076, 1.000000000000000000, 0.9330127018922194093, 0.9330127018922194093 ) ) 
 REPRESENTATION_ITEM ( '' )  );
#17426 = CARTESIAN_POINT ( 'NONE',  ( 4.175813232069147674, -2.061359961916367833, 3.570380186727398542 ) ) ;
#17427 = CARTESIAN_POINT ( 'NONE',  ( 0.6666666666666689611, 4.233901974057261874, -3.300726591567082480 ) ) ;
#17428 = CARTESIAN_POINT ( 'NONE',  ( -85.15643035624999868, -32.99062499938548854, 98.40857419181659793 ) ) ;
#17429 = CARTESIAN_POINT ( 'NONE',  ( 235.3564303562499447, -30.77812499938547575, -51.59142580818350865 ) ) ;
#17430 = EDGE_LOOP ( 'NONE', ( #6001, #12473, #18874, #2538 ) ) ;
#17431 = AXIS2_PLACEMENT_3D ( 'NONE', #14597, #4539, #19015 ) ;
#17432 = CARTESIAN_POINT ( 'NONE',  ( -81.02178482187500208, -33.14062499938548711, 102.3871387122750889 ) ) ;
#17433 = DIRECTION ( 'NONE',  ( 0.000000000000000000, 0.000000000000000000, -1.000000000000000000 ) ) ;
#17434 = CARTESIAN_POINT ( 'NONE',  ( 79.64356964374999848, -33.96562499938548285, 99.99999999999998579 ) ) ;
#17435 = CARTESIAN_POINT ( 'NONE',  ( 82.65333140691205926, -34.99995246259152282, -97.01071553687880566 ) ) ;
#17436 = AXIS2_PLACEMENT_3D ( 'NONE', #11255, #724, #15755 ) ;
#17437 = CARTESIAN_POINT ( 'NONE',  ( 235.3564303562499447, -32.12812499938547717, -51.59142580818350154 ) ) ;
#17438 = CARTESIAN_POINT ( 'NONE',  ( -85.15643035625001289, -32.91562499938548569, 101.5914258081833879 ) ) ;
#17439 = CARTESIAN_POINT ( 'NONE',  ( -85.15643035625001289, -34.79062499938548569, -101.5914258081833879 ) ) ;
#17440 = CARTESIAN_POINT ( 'NONE',  ( 82.39999999999999147, -33.17812499938548854, 96.81714838363319586 ) ) ;
#17441 = CARTESIAN_POINT ( 'NONE',  ( 81.02178482187500208, -34.15312499938548285, -102.3871387122750889 ) ) ;
#17442 = CARTESIAN_POINT ( 'NONE',  ( 233.9782151781249411, -32.69062499938547717, -47.61286128772501769 ) ) ;
#17443 = CARTESIAN_POINT ( 'NONE',  ( -79.64356964374999848, -32.61562499938548854, 99.99999999999998579 ) ) ;
#17444 = CARTESIAN_POINT ( 'NONE',  ( 79.64356964374999848, -30.36562499938548498, -99.99999999999998579 ) ) ;
#17445 = VERTEX_POINT ( 'NONE', #5884 ) ;
#17446 = CARTESIAN_POINT ( 'NONE',  ( 79.64356964374999848, -34.52812499938548285, 99.99999999999998579 ) ) ;
#17447 = CARTESIAN_POINT ( 'NONE',  ( 3.951447005078451813, 1.347150628109125892, 3.500000000000000444 ) ) ;
#17448 = CARTESIAN_POINT ( 'NONE',  ( -85.40000000000000568, -32.73750000000000426, 98.26794919243111792 ) ) ;
#17449 = CARTESIAN_POINT ( 'NONE',  ( -81.02178482187500208, -34.04062499938548569, 102.3871387122750889 ) ) ;
#17450 = CARTESIAN_POINT ( 'NONE',  ( -85.15643035625001289, -30.14062499938548711, 99.99999999999998579 ) ) ;
#17451 = ORIENTED_EDGE ( 'NONE', *, *, #4946, .T. ) ;
#17452 = LINE ( 'NONE', #15888, #4948 ) ;
#17453 = CARTESIAN_POINT ( 'NONE',  ( 235.3564303562499447, -33.55312499938548143, 101.5914258081833879 ) ) ;
#17454 = CARTESIAN_POINT ( 'NONE',  ( 79.67114894419047744, -35.00000000000000711, -99.22311565912301035 ) ) ;
#17455 = CARTESIAN_POINT ( 'NONE',  ( -82.39999999999999147, -31.23356250001229384, 103.4641016151377499 ) ) ;
#17456 =( BOUNDED_CURVE ( )  B_SPLINE_CURVE ( 2, ( #14322, #12769, #14413, #2217, #961, #11497, #18637, #7099, #1141 ),
 .UNSPECIFIED., .F., .F. ) 
 B_SPLINE_CURVE_WITH_KNOTS ( ( 3, 2, 2, 2, 3 ),
 ( 0.4791666666666666297, 0.4861111111111111049, 0.5000000000000000000, 0.5138888888888888395, 0.5208333333333334814 ),
 .UNSPECIFIED. ) 
 CURVE ( )  GEOMETRIC_REPRESENTATION_ITEM ( )  RATIONAL_B_SPLINE_CURVE ( ( 0.9330127018922194093, 0.9330127018922190762, 1.000000000000000000, 0.8660254037844387076, 1.000000000000000000, 0.8660254037844387076, 1.000000000000000000, 0.9330127018922177440, 0.9330127018922194093 ) ) 
 REPRESENTATION_ITEM ( '' )  );
#17457 = CARTESIAN_POINT ( 'NONE',  ( -83.20384757729335945, -34.40759618943233988, 102.9999999999999858 ) ) ;
#17458 = CARTESIAN_POINT ( 'NONE',  ( -82.65333140691201663, -34.99995246259153703, 97.01071553687880566 ) ) ;
#17459 = CARTESIAN_POINT ( 'NONE',  ( -81.59615242270662350, -33.41115380933863577, -96.99999999999998579 ) ) ;
#17460 = CARTESIAN_POINT ( 'NONE',  ( 230.2593261479345585, -31.99999999999999289, 98.53339280468536288 ) ) ;
#17461 = CARTESIAN_POINT ( 'NONE',  ( 82.39999999999999147, -30.36562499938549209, 103.1828516163667899 ) ) ;
#17462 = CARTESIAN_POINT ( 'NONE',  ( 0.000000000000000000, -3.031088913245531202, 1.750000000000006661 ) ) ;
#17463 = CARTESIAN_POINT ( 'NONE',  ( -83.90000000000000568, -32.71874999877096712, -102.5980762113533018 ) ) ;
#17464 = CARTESIAN_POINT ( 'NONE',  ( 79.64356964375001269, -34.11562499938548854, -101.5914258081833879 ) ) ;
#17465 = CARTESIAN_POINT ( 'NONE',  ( 249.9999999999999716, -35.00000000000000000, 150.0000000000000000 ) ) ;
#17466 = EDGE_LOOP ( 'NONE', ( #12869, #16020, #13826, #10166 ) ) ;
#17467 = CARTESIAN_POINT ( 'NONE',  ( 82.39999999999999147, -32.98124999877096997, 96.53589838486223584 ) ) ;
#17468 = CARTESIAN_POINT ( 'NONE',  ( 231.2217848218749339, -35.12812499938548427, 102.3871387122750889 ) ) ;
#17469 = CARTESIAN_POINT ( 'NONE',  ( 231.2217848218749339, -33.77812499938547575, -47.61286128772501769 ) ) ;
#17470 = ADVANCED_FACE ( 'NONE', ( #14855 ), #7338, .T. ) ;
#17471 = EDGE_CURVE ( 'NONE', #7231, #19103, #1481, .T. ) ;
#17472 = FACE_OUTER_BOUND ( 'NONE', #14910, .T. ) ;
#17473 = CARTESIAN_POINT ( 'NONE',  ( 82.40000000000001990, -34.16250000000000853, 103.0000000000000000 ) ) ;
#17474 = ORIENTED_EDGE ( 'NONE', *, *, #757, .F. ) ;
#17475 = CARTESIAN_POINT ( 'NONE',  ( -85.15643035625001289, -33.29062499938547859, -99.99999999999998579 ) ) ;
#17476 = DIRECTION ( 'NONE',  ( 1.735459783503185124E-31, 3.491481338843133355E-15, 1.000000000000000000 ) ) ;
#17477 = ORIENTED_EDGE ( 'NONE', *, *, #12861, .F. ) ;
#17478 = DIRECTION ( 'NONE',  ( 1.000000000000000000, 0.000000000000000000, -0.000000000000000000 ) ) ;
#17479 = CARTESIAN_POINT ( 'NONE',  ( -79.64356964375001269, -31.41562499938548569, -98.40857419181659793 ) ) ;
#17480 = CARTESIAN_POINT ( 'NONE',  ( 84.01447415327271528, -35.02670941564510088, 102.7431224211893692 ) ) ;
#17481 = CARTESIAN_POINT ( 'NONE',  ( -83.20384757729338787, -34.59240381056766722, 97.00000000000000000 ) ) ;
#17482 = CARTESIAN_POINT ( 'NONE',  ( -85.40000000000000568, -34.44374999877096855, 99.99999999999998579 ) ) ;
#17483 = CARTESIAN_POINT ( 'NONE',  ( -85.15643035624999868, -31.11562499938548854, 101.5914258081833879 ) ) ;
#17484 = ADVANCED_FACE ( 'NONE', ( #2721 ), #7600, .T. ) ;
#17485 = DIRECTION ( 'NONE',  ( 0.000000000000000000, 0.000000000000000000, -1.000000000000000000 ) ) ;
#17486 = EDGE_CURVE ( 'NONE', #10662, #14886, #7309, .T. ) ;
#17487 = CARTESIAN_POINT ( 'NONE',  ( -94.79999999999999716, -5.200000000000000178, 150.0000000000000000 ) ) ;
#17488 = ADVANCED_FACE ( 'NONE', ( #12094 ), #16501, .T. ) ;
#17489 = CARTESIAN_POINT ( 'NONE',  ( 82.39999999999999147, -32.98124999877096997, -103.4641016151377499 ) ) ;
#17490 = CARTESIAN_POINT ( 'NONE',  ( 229.5999999999999375, -32.24999999999999289, 99.99999999999998579 ) ) ;
#17491 = ORIENTED_EDGE ( 'NONE', *, *, #10075, .T. ) ;
#17492 = CARTESIAN_POINT ( 'NONE',  ( 230.5523683116323355, -32.00000000000000000, -48.15470523285603832 ) ) ;
#17493 = CARTESIAN_POINT ( 'NONE',  ( 234.0999999999999375, -33.39374999877096428, 102.5980762113533018 ) ) ;
#17494 = CARTESIAN_POINT ( 'NONE',  ( 231.0999999999999375, -31.21874999877096357, -47.40192378864679768 ) ) ;
#17495 = CARTESIAN_POINT ( 'NONE',  ( -84.69814161231455785, -35.39427329483935836, 98.07164704222790874 ) ) ;
#17496 = CARTESIAN_POINT ( 'NONE',  ( 112.8867513459481984, 10.19999999999997264, -150.0000000000000000 ) ) ;
#17497 = ORIENTED_EDGE ( 'NONE', *, *, #15097, .T. ) ;
#17498 = ORIENTED_EDGE ( 'NONE', *, *, #7465, .F. ) ;
#17499 = CARTESIAN_POINT ( 'NONE',  ( -4.207491450040567571, 2.029819825146470524, -3.671670828759566074 ) ) ;
#17500 = CARTESIAN_POINT ( 'NONE',  ( -83.90000000000000568, -32.11874999877097281, 102.5980762113533018 ) ) ;
#17501 = ORIENTED_EDGE ( 'NONE', *, *, #18203, .T. ) ;
#17502 = DIRECTION ( 'NONE',  ( 1.000000000000000000, 0.000000000000000000, 0.000000000000000000 ) ) ;
#17503 = CARTESIAN_POINT ( 'NONE',  ( 82.39999999999999147, -31.68750000000000355, -103.4641016151377499 ) ) ;
#17504 = CARTESIAN_POINT ( 'NONE',  ( -82.39999999999999147, -33.65624999877097423, -103.0000000000000000 ) ) ;
#17505 = CARTESIAN_POINT ( 'NONE',  ( -79.64356964375001269, -32.76562499938548711, 101.5914258081833879 ) ) ;
#17506 = CARTESIAN_POINT ( 'NONE',  ( -80.90000000000000568, -31.50000000000000000, 97.40192378864668399 ) ) ;
#17507 = CARTESIAN_POINT ( 'NONE',  ( 235.2218879900010506, -35.00000000000000000, -49.14934632385183022 ) ) ;
#17508 = DIRECTION ( 'NONE',  ( 0.000000000000000000, 0.000000000000000000, 1.000000000000000000 ) ) ;
#17509 = DIRECTION ( 'NONE',  ( -0.000000000000000000, -0.000000000000000000, -1.000000000000000000 ) ) ;
#17510 = CARTESIAN_POINT ( 'NONE',  ( -2.000000000000002665, -3.464101615137770374, -3.142992957459237680 ) ) ;
#17511 = CARTESIAN_POINT ( 'NONE',  ( -1.959187206999195895E-15, 3.202582148906728765, 1.452965002680430828 ) ) ;
#17512 =( BOUNDED_CURVE ( )  B_SPLINE_CURVE ( 1, ( #17601, #4214 ),
 .UNSPECIFIED., .F., .F. ) 
 B_SPLINE_CURVE_WITH_KNOTS ( ( 2, 2 ),
 ( 0.000000000000000000, 1.000000000000000000 ),
 .UNSPECIFIED. ) 
 CURVE ( )  GEOMETRIC_REPRESENTATION_ITEM ( )  RATIONAL_B_SPLINE_CURVE ( ( 0.9401539157124900736, 0.9401539157124900736 ) ) 
 REPRESENTATION_ITEM ( '' )  );
#17513 = CARTESIAN_POINT ( 'NONE',  ( -81.59615242270662350, -31.03259618943233988, 96.99999999999998579 ) ) ;
#17514 = ORIENTED_EDGE ( 'NONE', *, *, #1759, .F. ) ;
#17515 = CARTESIAN_POINT ( 'NONE',  ( -83.77821517812500929, -31.86562499938548498, -97.61286128772489690 ) ) ;
#17516 = CARTESIAN_POINT ( 'NONE',  ( 234.9631320699431001, -35.00000000000000000, 98.35371953419910085 ) ) ;
#17517 = CARTESIAN_POINT ( 'NONE',  ( 69.99999999999998579, -34.99999999999999289, -150.0000000000000000 ) ) ;
#17518 = CARTESIAN_POINT ( 'NONE',  ( 229.8435696437499587, -34.34062499938547575, 98.40857419181659793 ) ) ;
#17519 = CARTESIAN_POINT ( 'NONE',  ( -82.39999999999999147, -32.84062499938548996, 103.1828516163667899 ) ) ;
#17520 = CARTESIAN_POINT ( 'NONE',  ( 79.39999999999999147, -32.43750000000000000, 101.7320508075688963 ) ) ;
#17521 = CARTESIAN_POINT ( 'NONE',  ( 229.8435696437499303, -34.75312499938547717, -50.00000000000011369 ) ) ;
#17522 = ORIENTED_EDGE ( 'NONE', *, *, #13405, .F. ) ;
#17523 = EDGE_CURVE ( 'NONE', #2832, #11219, #4635, .T. ) ;
#17524 = CARTESIAN_POINT ( 'NONE',  ( -85.15643035625001289, -32.84062499938548285, 99.99999999999998579 ) ) ;
#17525 = DIRECTION ( 'NONE',  ( -0.000000000000000000, -1.000000000000000000, -0.000000000000000000 ) ) ;
#17526 = CARTESIAN_POINT ( 'NONE',  ( 80.90000000000000568, -30.30000000000000426, 97.40192378864668399 ) ) ;
#17527 = FACE_OUTER_BOUND ( 'NONE', #449, .T. ) ;
#17528 = CARTESIAN_POINT ( 'NONE',  ( 232.5999999999999375, -30.47812499938547859, 103.1828516163667899 ) ) ;
#17529 = CARTESIAN_POINT ( 'NONE',  ( 229.8435696437499587, -32.35312499938547859, -48.40857419181671162 ) ) ;
#17530 = DIRECTION ( 'NONE',  ( 1.000000000000000000, 0.000000000000000000, 0.000000000000000000 ) ) ;
#17531 = CARTESIAN_POINT ( 'NONE',  ( -79.64356964374998427, -33.14062499938548711, -101.5914258081833879 ) ) ;
#17532 = CARTESIAN_POINT ( 'NONE',  ( 85.15643035624999868, -34.15312499938548285, 98.40857419181659793 ) ) ;
#17533 = CARTESIAN_POINT ( 'NONE',  ( 85.15643035624999868, -35.16562499938547859, -101.5914258081833879 ) ) ;
#17534 = CARTESIAN_POINT ( 'NONE',  ( 231.0999999999999375, -31.27499999999999858, -47.40192378864679768 ) ) ;
#17535 = CARTESIAN_POINT ( 'NONE',  ( -85.15643035625001289, -32.39062499938548711, 99.99999999999998579 ) ) ;
#17536 = CARTESIAN_POINT ( 'NONE',  ( 3.972073812946708582, -0.6951863858492246528, -3.565770933504603057 ) ) ;
#17537 = EDGE_LOOP ( 'NONE', ( #6989, #18850, #9970, #4077 ) ) ;
#17538 = CARTESIAN_POINT ( 'NONE',  ( 82.39999999999999147, -34.41562499938547859, 103.1828516163667899 ) ) ;
#17539 = CARTESIAN_POINT ( 'NONE',  ( 0.5276280594147412240, -4.314175951381924889, -3.320322319201654881 ) ) ;
#17540 = CARTESIAN_POINT ( 'NONE',  ( -82.39999999999999147, -33.93750000000000000, 103.4641016151377499 ) ) ;
#17541 = CARTESIAN_POINT ( 'NONE',  ( -79.64356964375001269, -32.12812499938548427, 98.40857419181659793 ) ) ;
#17542 = CARTESIAN_POINT ( 'NONE',  ( -82.39999999999999147, -30.25312499938548783, 96.81714838363319586 ) ) ;
#17543 = ORIENTED_EDGE ( 'NONE', *, *, #2702, .T. ) ;
#17544 = CARTESIAN_POINT ( 'NONE',  ( -83.90000000000000568, -30.52500000000000213, 97.40192378864668399 ) ) ;
#17545 = VECTOR ( 'NONE', #3989, 1000.000000000000000 ) ;
#17546 = CIRCLE ( 'NONE', #7553, 4.000000000000000000 ) ;
#17547 = CARTESIAN_POINT ( 'NONE',  ( 231.2217848218749339, -32.91562499938547148, 97.61286128772489690 ) ) ;
#17548 = DIRECTION ( 'NONE',  ( 1.000000000000000000, -0.000000000000000000, -0.000000000000000000 ) ) ;
#17549 = CARTESIAN_POINT ( 'NONE',  ( 82.40000000000000568, -32.08124999877097139, -102.9999999999999858 ) ) ;
#17550 = CARTESIAN_POINT ( 'NONE',  ( 4.052424581287633387, 2.393186648132967775, -2.990837702970182477 ) ) ;
#17551 = CARTESIAN_POINT ( 'NONE',  ( 1.411581201560190495E-15, 4.862606272033091592, -3.745885042887436622 ) ) ;
#17552 = CARTESIAN_POINT ( 'NONE',  ( -79.64356964375001269, -30.40312499938548285, 101.5914258081833879 ) ) ;
#17553 = CARTESIAN_POINT ( 'NONE',  ( 111.5000000000000142, 12.69999999999998508, 50.00000000000001421 ) ) ;
#17554 = CARTESIAN_POINT ( 'NONE',  ( 85.15643035624999868, -32.54062499938548569, 101.5914258081833879 ) ) ;
#17555 = CARTESIAN_POINT ( 'NONE',  ( 109.9999999999999432, -29.80000000000002558, -150.0000000000000000 ) ) ;
#17556 = EDGE_CURVE ( 'NONE', #14982, #18033, #7505, .T. ) ;
#17557 = CARTESIAN_POINT ( 'NONE',  ( -85.40000000000000568, -32.64374999877097139, -99.99999999999998579 ) ) ;
#17558 = CARTESIAN_POINT ( 'NONE',  ( 83.77821517812500929, -34.22812499938549280, -102.3871387122750889 ) ) ;
#17559 = DIRECTION ( 'NONE',  ( 0.000000000000000000, 0.000000000000000000, 1.000000000000000000 ) ) ;
#17560 = AXIS2_PLACEMENT_3D ( 'NONE', #2378, #14572, #11366 ) ;
#17561 = CONICAL_SURFACE ( 'NONE', #9125, 2.055000000000000160, 0.7853981633974439491 ) ;
#17562 = VERTEX_POINT ( 'NONE', #10342 ) ;
#17563 = CARTESIAN_POINT ( 'NONE',  ( 85.40000000000000568, -33.58124999877097139, 101.7320508075688679 ) ) ;
#17564 = CARTESIAN_POINT ( 'NONE',  ( 231.2217848218749339, -34.82812499938548001, 97.61286128772489690 ) ) ;
#17565 = CARTESIAN_POINT ( 'NONE',  ( 85.40000000000000568, -32.60624999877096997, 98.26794919243111792 ) ) ;
#17566 = CARTESIAN_POINT ( 'NONE',  ( -85.40000000000000568, -30.39374999877097139, 99.99999999999998579 ) ) ;
#17567 = CARTESIAN_POINT ( 'NONE',  ( 231.7961524227065979, -32.60759618943232852, -47.00000000000010658 ) ) ;
#17568 = VERTEX_POINT ( 'NONE', #16306 ) ;
#17569 = CARTESIAN_POINT ( 'NONE',  ( -85.15643035625001289, -34.64062499938548711, -99.99999999999998579 ) ) ;
#17570 = CARTESIAN_POINT ( 'NONE',  ( 82.40000000000000568, -30.00000000000000355, 96.99999999999998579 ) ) ;
#17571 = ORIENTED_EDGE ( 'NONE', *, *, #3031, .T. ) ;
#17572 = APPLICATION_CONTEXT ( 'automotive_design' ) ;
#17573 = CARTESIAN_POINT ( 'NONE',  ( 79.77811200999867935, -34.99999999999999289, 99.14934632385235602 ) ) ;
#17574 = CARTESIAN_POINT ( 'NONE',  ( -85.15643035624999868, -30.74062499938548143, -101.5914258081833879 ) ) ;
#17575 = CARTESIAN_POINT ( 'NONE',  ( -79.39999999999999147, -30.65624999877096712, -98.26794919243113213 ) ) ;
#17576 = CARTESIAN_POINT ( 'NONE',  ( 79.77811200999867935, -34.99999999999999289, 99.14934632385235602 ) ) ;
#17577 = CARTESIAN_POINT ( 'NONE',  ( -79.39999999999999147, -34.66874999877096997, 99.99999999999998579 ) ) ;
#17578 = CARTESIAN_POINT ( 'NONE',  ( -82.39999999999999147, -31.04062499938548569, 103.1828516163667899 ) ) ;
#17579 = CARTESIAN_POINT ( 'NONE',  ( -80.90000000000000568, -30.69374999877097210, 102.5980762113533018 ) ) ;
#17580 = CARTESIAN_POINT ( 'NONE',  ( 231.9680721332268831, -35.00000000000000000, 102.6890373435399937 ) ) ;
#17581 = CARTESIAN_POINT ( 'NONE',  ( 80.90000000000000568, -31.14374999877097139, -102.5980762113533018 ) ) ;
#17582 = CARTESIAN_POINT ( 'NONE',  ( 235.5999999999999375, -31.12499999999999645, 99.99999999999998579 ) ) ;
#17583 = ORIENTED_EDGE ( 'NONE', *, *, #539, .T. ) ;
#17584 = CARTESIAN_POINT ( 'NONE',  ( 79.64356964374998427, -34.37812499938548427, -98.40857419181659793 ) ) ;
#17585 = CARTESIAN_POINT ( 'NONE',  ( 234.0999999999999375, -32.34374999877096002, 97.40192378864668399 ) ) ;
#17586 = CARTESIAN_POINT ( 'NONE',  ( 229.5999999999999375, -32.68124999877096570, -51.73205080756898866 ) ) ;
#17587 = CARTESIAN_POINT ( 'NONE',  ( 232.5999999999999659, -32.53124999877096712, 102.9999999999999858 ) ) ;
#17588 = CARTESIAN_POINT ( 'NONE',  ( -82.39999999999999147, -32.05312499938548854, 96.81714838363319586 ) ) ;
#17589 = ORIENTED_EDGE ( 'NONE', *, *, #2798, .F. ) ;
#17590 = ORIENTED_EDGE ( 'NONE', *, *, #15435, .T. ) ;
#17591 = CARTESIAN_POINT ( 'NONE',  ( -82.40000000000001990, -32.13750000000000284, 103.0000000000000000 ) ) ;
#17592 = PLANE ( 'NONE',  #1930 ) ;
#17593 = ORIENTED_EDGE ( 'NONE', *, *, #13422, .F. ) ;
#17594 = DIRECTION ( 'NONE',  ( -0.000000000000000000, -0.000000000000000000, -1.000000000000000000 ) ) ;
#17595 = CARTESIAN_POINT ( 'NONE',  ( 82.39999999999999147, -31.91250000000000497, -96.53589838486223584 ) ) ;
#17596 = DIRECTION ( 'NONE',  ( 0.000000000000000000, 0.8660254037844375974, -0.5000000000000018874 ) ) ;
#17597 = B_SPLINE_CURVE_WITH_KNOTS ( 'NONE', 3,
 ( #16698, #4886, #12302, #1940, #15038, #398 ),
 .UNSPECIFIED., .F., .F.,
 ( 4, 2, 4 ),
 ( 0.000000000000000000, 0.0002095117440864783663, 0.0004190234881729567326 ),
 .UNSPECIFIED. ) ;
#17598 = CARTESIAN_POINT ( 'NONE',  ( -82.39999999999999147, -32.39062499938548001, 103.1828516163667899 ) ) ;
#17599 = CARTESIAN_POINT ( 'NONE',  ( -83.90000000000000568, -32.17500000000000426, 102.5980762113533018 ) ) ;
#17600 = CARTESIAN_POINT ( 'NONE',  ( 234.0999999999999375, -32.34374999877096002, -52.59807621135342970 ) ) ;
#17601 = CARTESIAN_POINT ( 'NONE',  ( -84.70833260042415702, -35.00006955123599539, 98.08383195543535749 ) ) ;
#17602 = ADVANCED_FACE ( 'NONE', ( #14728 ), #9291, .T. ) ;
#17603 = CARTESIAN_POINT ( 'NONE',  ( 81.48596794228855344, -35.00000000000000000, 102.8136019330778907 ) ) ;
#17604 = CARTESIAN_POINT ( 'NONE',  ( 0.000000000000000000, 3.031088913245533867, 1.750000000000002887 ) ) ;
#17605 = CARTESIAN_POINT ( 'NONE',  ( 233.9782151781249411, -30.29062499938547859, 97.61286128772489690 ) ) ;
#17606 = VERTEX_POINT ( 'NONE', #2916 ) ;
#17607 = CARTESIAN_POINT ( 'NONE',  ( -79.64356964375001269, -35.01562499938548711, -98.40857419181659793 ) ) ;
#17608 = CARTESIAN_POINT ( 'NONE',  ( 0.000000000000000000, 0.000000000000000000, -4.000000000000000000 ) ) ;
#17609 = DIRECTION ( 'NONE',  ( 1.000000000000000000, -1.387778780781445676E-15, -2.407412430484046130E-31 ) ) ;
#17610 = CARTESIAN_POINT ( 'NONE',  ( 229.8435696437499303, -33.85312499938548569, 99.99999999999998579 ) ) ;
#17611 = CARTESIAN_POINT ( 'NONE',  ( -82.39999999999999147, -31.82812499938548356, 103.1828516163667899 ) ) ;
#17612 = CARTESIAN_POINT ( 'NONE',  ( 82.39999999999999147, -32.81250000000000000, -97.00000000000000000 ) ) ;
#17613 = ADVANCED_FACE ( 'NONE', ( #3104 ), #17965, .T. ) ;
#17614 = CARTESIAN_POINT ( 'NONE',  ( 231.2217848218749339, -33.66562499938547859, -47.61286128772501769 ) ) ;
#17616 = EDGE_CURVE ( 'NONE', #5441, #677, #17423, .T. ) ;
#17615 = ORIENTED_EDGE ( 'NONE', *, *, #10541, .T. ) ;
#17617 = ORIENTED_EDGE ( 'NONE', *, *, #5453, .F. ) ;
#17618 = CARTESIAN_POINT ( 'NONE',  ( -85.15643035624999868, -34.60312499938548569, 101.5914258081833879 ) ) ;
#17619 = EDGE_CURVE ( 'NONE', #12080, #4350, #17729, .T. ) ;
#17620 = LINE ( 'NONE', #13213, #16307 ) ;
#17621 = CARTESIAN_POINT ( 'NONE',  ( 82.39999999999999147, -30.78750000000000497, 96.53589838486223584 ) ) ;
#17622 = FACE_OUTER_BOUND ( 'NONE', #8470, .T. ) ;
#17623 = CARTESIAN_POINT ( 'NONE',  ( 235.3564303562499447, -30.81562499938547717, 99.99999999999998579 ) ) ;
#17624 =( BOUNDED_CURVE ( )  B_SPLINE_CURVE ( 2, ( #15793, #8074, #18631, #2399, #6613, #12563, #5251, #11197, #11390 ),
 .UNSPECIFIED., .F., .F. ) 
 B_SPLINE_CURVE_WITH_KNOTS ( ( 3, 2, 2, 2, 3 ),
 ( 0.5208333333333333703, 0.5277777777777777901, 0.5416666666666666297, 0.5555555555555555802, 0.5625000000000000000 ),
 .UNSPECIFIED. ) 
 CURVE ( )  GEOMETRIC_REPRESENTATION_ITEM ( )  RATIONAL_B_SPLINE_CURVE ( ( 0.9330127018922192983, 0.9330127018922198534, 1.000000000000000000, 0.8660254037844387076, 1.000000000000000000, 0.8660254037844387076, 1.000000000000000000, 0.9330127018922194093, 0.9330127018922194093 ) ) 
 REPRESENTATION_ITEM ( '' )  );
#17625 = CARTESIAN_POINT ( 'NONE',  ( 232.5999999999999943, -34.52812499938547575, -46.81714838363331666 ) ) ;
#17626 = LINE ( 'NONE', #1762, #5222 ) ;
#17627 = CARTESIAN_POINT ( 'NONE',  ( 82.39999999999999147, -33.85312499938547859, 103.1828516163667899 ) ) ;
#17628 = CARTESIAN_POINT ( 'NONE',  ( 79.64356964375001269, -31.30312499938548854, -101.5914258081833879 ) ) ;
#17629 = ADVANCED_FACE ( 'NONE', ( #13462 ), #13370, .T. ) ;
#17630 = CARTESIAN_POINT ( 'NONE',  ( 231.7447645400923193, -35.19352049914630953, -53.26902605122407408 ) ) ;
#17631 = CARTESIAN_POINT ( 'NONE',  ( -85.15643035625001289, -34.22812499938548569, 98.40857419181659793 ) ) ;
#17632 = CARTESIAN_POINT ( 'NONE',  ( 81.02178482187500208, -30.44062499938548783, -102.3871387122750889 ) ) ;
#17633 = B_SPLINE_CURVE_WITH_KNOTS ( 'NONE', 3,
 ( #1997, #12449, #6308, #5036, #6595, #14009, #16749, #18416, #13812, #12543, #1802, #6694, #453, #7954, #16947, #3367 ),
 .UNSPECIFIED., .F., .F.,
 ( 4, 2, 2, 2, 2, 2, 2, 4 ),
 ( 0.000000000000000000, 0.0005391024520904312426, 0.001078204904180862485, 0.002156409808361685505, 0.002695512260452097124, 0.003234614712542508742, 0.003773717164632920361, 0.004312819616723331979 ),
 .UNSPECIFIED. ) ;
#17634 = VERTEX_POINT ( 'NONE', #193 ) ;
#17635 = CARTESIAN_POINT ( 'NONE',  ( 81.02178482187500208, -34.15312499938548285, 97.61286128772489690 ) ) ;
#17636 = DIRECTION ( 'NONE',  ( 0.000000000000000000, 0.000000000000000000, -1.000000000000000000 ) ) ;
#17637 = CARTESIAN_POINT ( 'NONE',  ( 231.2217848218749339, -31.67812499938547788, -52.38713871227520968 ) ) ;
#17638 = CARTESIAN_POINT ( 'NONE',  ( -85.15643035624999868, -34.22812499938547859, 98.40857419181659793 ) ) ;
#17639 = EDGE_LOOP ( 'NONE', ( #3257, #1465, #305, #7412, #1938 ) ) ;
#17640 = CARTESIAN_POINT ( 'NONE',  ( -82.40000000000000568, -34.10624999877096997, 96.99999999999998579 ) ) ;
#17641 = B_SPLINE_CURVE_WITH_KNOTS ( 'NONE', 3,
 ( #17235, #18512, #10883, #8049, #3745, #5330, #13905, #16852, #9711, #3557, #11174, #3456, #14005, #15580, #14196, #9619 ),
 .UNSPECIFIED., .F., .F.,
 ( 4, 2, 2, 2, 2, 2, 2, 4 ),
 ( 0.000000000000000000, 0.0005391024520904608413, 0.001078204904180921683, 0.002156409808361816477, 0.002695512260452254550, 0.003234614712542692189, 0.003773717164633130262, 0.004312819616723567902 ),
 .UNSPECIFIED. ) ;
#17642 = AXIS2_PLACEMENT_3D ( 'NONE', #7118, #13453, #11604 ) ;
#17643 = CARTESIAN_POINT ( 'NONE',  ( 232.5999999999999943, -32.50312499938547717, 96.81714838363319586 ) ) ;
#17644 = CYLINDRICAL_SURFACE ( 'NONE', #3928, 2.500000000000000444 ) ;
#17645 = CARTESIAN_POINT ( 'NONE',  ( -85.40000000000000568, -33.55856250001229313, 101.7320508075688679 ) ) ;
#17646 = EDGE_CURVE ( 'NONE', #3049, #10326, #13451, .T. ) ;
#17647 = CARTESIAN_POINT ( 'NONE',  ( 232.5999999999999659, -32.13749999999999574, 103.0000000000000000 ) ) ;
#17648 = CARTESIAN_POINT ( 'NONE',  ( -79.39999999999999147, -32.45624999877097139, 101.7320508075688537 ) ) ;
#17649 = CARTESIAN_POINT ( 'NONE',  ( -85.15643035625001289, -31.49062499938548498, 99.99999999999998579 ) ) ;
#17650 = CARTESIAN_POINT ( 'NONE',  ( -83.90000000000000568, -32.71874999877096712, 97.40192378864668399 ) ) ;
#17651 = CARTESIAN_POINT ( 'NONE',  ( 79.64356964375001269, -32.76562499938548711, 98.40857419181659793 ) ) ;
#17652 = CARTESIAN_POINT ( 'NONE',  ( 232.5999999999999375, -33.71249999999999147, -53.00000000000010658 ) ) ;
#17653 = CARTESIAN_POINT ( 'NONE',  ( -80.90000000000000568, -32.40000000000000568, -102.5980762113533018 ) ) ;
#17654 = CARTESIAN_POINT ( 'NONE',  ( 81.02178482187500208, -33.55312499938548854, -97.61286128772489690 ) ) ;
#17655 = CARTESIAN_POINT ( 'NONE',  ( -79.64356964374999848, -30.92812499938548498, -99.99999999999998579 ) ) ;
#17656 = VECTOR ( 'NONE', #18225, 1000.000000000000000 ) ;
#17657 = ORIENTED_EDGE ( 'NONE', *, *, #12497, .T. ) ;
#17658 = CARTESIAN_POINT ( 'NONE',  ( 80.90000000000000568, -33.84374999877096712, 97.40192378864668399 ) ) ;
#17659 = CARTESIAN_POINT ( 'NONE',  ( 232.1454721953968772, -35.00000000000000711, -47.27546421900289886 ) ) ;
#17660 = CARTESIAN_POINT ( 'NONE',  ( 102.9999999999999858, -5.200000000000008171, -100.0000000000000000 ) ) ;
#17661 = CARTESIAN_POINT ( 'NONE',  ( -79.64356964374999848, -34.86562499938548143, 99.99999999999998579 ) ) ;
#17662 = CARTESIAN_POINT ( 'NONE',  ( -85.23110191009446623, -35.00000000000000000, -100.8575180188184675 ) ) ;
#17663 = VERTEX_POINT ( 'NONE', #8966 ) ;
#17664 = CARTESIAN_POINT ( 'NONE',  ( -85.15643035625001289, -35.09062499938548285, -99.99999999999998579 ) ) ;
#17665 = CARTESIAN_POINT ( 'NONE',  ( 4.000000000000000000, -1.677850389431204459, -3.535268758346977513 ) ) ;
#17666 = ORIENTED_EDGE ( 'NONE', *, *, #17833, .F. ) ;
#17667 = CYLINDRICAL_SURFACE ( 'NONE', #17642, 3.000000000000002665 ) ;
#17668 = CARTESIAN_POINT ( 'NONE',  ( -80.90000000000000568, -35.04374999877096997, -102.5980762113533018 ) ) ;
#17669 = CARTESIAN_POINT ( 'NONE',  ( -82.61711639270095020, -32.00000000000000000, -102.8399189874719042 ) ) ;
#17670 = CARTESIAN_POINT ( 'NONE',  ( -79.39999999999999147, -31.06874999877096855, -99.99999999999998579 ) ) ;
#17671 = CARTESIAN_POINT ( 'NONE',  ( 232.5999999999999375, -32.61562499938548143, 96.81714838363319586 ) ) ;
#17672 = CARTESIAN_POINT ( 'NONE',  ( -85.40000000000000568, -34.85624999877096997, 101.7320508075688679 ) ) ;
#17673 = CARTESIAN_POINT ( 'NONE',  ( -82.39999999999999147, -33.96562499938548285, 96.81714838363319586 ) ) ;
#17674 = CARTESIAN_POINT ( 'NONE',  ( -79.64356964374999848, -34.86562499938548143, -99.99999999999998579 ) ) ;
#17675 = CARTESIAN_POINT ( 'NONE',  ( 94.79999999999995453, -5.200000000000000178, 150.0000000000000000 ) ) ;
#17676 = CARTESIAN_POINT ( 'NONE',  ( -82.40000000000000568, -30.00000000000000355, 103.0000000000000000 ) ) ;
#17677 = CARTESIAN_POINT ( 'NONE',  ( 79.39999999999999147, -30.65624999877096712, -101.7320508075688537 ) ) ;
#17678 = CARTESIAN_POINT ( 'NONE',  ( 231.0999999999999375, -30.82499999999999574, 102.5980762113533018 ) ) ;
#17679 = AXIS2_PLACEMENT_3D ( 'NONE', #17878, #4487, #10441 ) ;
#17680 = ORIENTED_EDGE ( 'NONE', *, *, #3467, .T. ) ;
#17681 = CARTESIAN_POINT ( 'NONE',  ( 117.5000000000000142, 12.69999999999998508, 30.20101012677667285 ) ) ;
#17682 =( NAMED_UNIT ( * ) PLANE_ANGLE_UNIT ( ) SI_UNIT ( $, .RADIAN. ) );
#17683 = CARTESIAN_POINT ( 'NONE',  ( 234.0999999999999375, -33.24374999877096570, 97.40192378864668399 ) ) ;
#17684 = CARTESIAN_POINT ( 'NONE',  ( 234.0999999999999375, -34.29374999877096286, -47.40192378864679768 ) ) ;
#17685 = CARTESIAN_POINT ( 'NONE',  ( -85.15643035625001289, -32.87812499938548427, 98.40857419181659793 ) ) ;
#17686 = ORIENTED_EDGE ( 'NONE', *, *, #14467, .F. ) ;
#17687 = EDGE_LOOP ( 'NONE', ( #13943, #17159, #17087, #1838 ) ) ;
#17688 = CARTESIAN_POINT ( 'NONE',  ( 81.59615242270665192, -34.18259618943233136, -97.00000000000000000 ) ) ;
#17689 = CARTESIAN_POINT ( 'NONE',  ( 99.99999999999997158, -5.200000000000008171, 150.0000000000000000 ) ) ;
#17690 = DIRECTION ( 'NONE',  ( 1.000000000000000000, -1.387778780781445478E-15, -2.407412430484046130E-31 ) ) ;
#17691 = EDGE_LOOP ( 'NONE', ( #10289, #16318, #1676, #18286 ) ) ;
#17692 = CARTESIAN_POINT ( 'NONE',  ( 1.999999999999998224, -3.464101615137772594, -3.142992957459239012 ) ) ;
#17693 = CARTESIAN_POINT ( 'NONE',  ( 85.40000000000000568, -34.91250000000000142, -101.7320508075688679 ) ) ;
#17694 = CARTESIAN_POINT ( 'NONE',  ( 0.3126073911696408136, 2.020725942163688060, 3.500000000000000000 ) ) ;
#17695 = CARTESIAN_POINT ( 'NONE',  ( 80.90000000000000568, -35.04374999877096997, 102.5980762113533018 ) ) ;
#17696 = CARTESIAN_POINT ( 'NONE',  ( -85.15643035625001289, -33.85312499938549280, 99.99999999999998579 ) ) ;
#17697 = CARTESIAN_POINT ( 'NONE',  ( -83.90000000000000568, -32.62500000000000000, 102.5980762113533018 ) ) ;
#17698 = AXIS2_PLACEMENT_3D ( 'NONE', #8110, #18379, #792 ) ;
#17699 = CARTESIAN_POINT ( 'NONE',  ( 230.7186334667984227, -32.00000000000000711, -52.01453922190813728 ) ) ;
#17700 = CARTESIAN_POINT ( 'NONE',  ( 81.70916641599873742, -34.99999999999999289, 102.8868501612598862 ) ) ;
#17701 = CARTESIAN_POINT ( 'NONE',  ( 83.20395887649176814, -35.00000000000001421, 97.36341917746361219 ) ) ;
#17702 = CARTESIAN_POINT ( 'NONE',  ( -83.90000000000000568, -34.51874999877097139, -102.5980762113533018 ) ) ;
#17703 = ORIENTED_EDGE ( 'NONE', *, *, #17168, .F. ) ;
#17704=STYLED_ITEM('',(#19350),#3102);
#17705 = SURFACE_STYLE_FILL_AREA ( #5784 ) ;
#17706 = CARTESIAN_POINT ( 'NONE',  ( -83.77821517812500929, -30.21562499938548285, -102.3871387122750889 ) ) ;
#17707 = CARTESIAN_POINT ( 'NONE',  ( 1.390230914382191596, 4.043987460488659202, -3.502507215260488582 ) ) ;
#17708 = ADVANCED_FACE ( 'NONE', ( #6143 ), #11707, .T. ) ;
#17709 = CARTESIAN_POINT ( 'NONE',  ( 0.000000000000000000, 0.000000000000000000, 0.000000000000000000 ) ) ;
#17710 = CARTESIAN_POINT ( 'NONE',  ( -85.40000000000000568, -34.95000000000000284, -99.99999999999998579 ) ) ;
#17711 = CARTESIAN_POINT ( 'NONE',  ( -81.02178482187500208, -30.44062499938548783, 102.3871387122750889 ) ) ;
#17712 = CARTESIAN_POINT ( 'NONE',  ( 80.90000000000000568, -33.30000000000000426, 102.5980762113533018 ) ) ;
#17713 = CARTESIAN_POINT ( 'NONE',  ( 235.3564303562499447, -33.92812499938548143, -51.59142580818350865 ) ) ;
#17714 = AXIS2_PLACEMENT_3D ( 'NONE', #5935, #14867, #3179 ) ;
#17715 = ADVANCED_FACE ( 'NONE', ( #16113 ), #1268, .F. ) ;
#17716 = VECTOR ( 'NONE', #18047, 1000.000000000000000 ) ;
#17717 = EDGE_CURVE ( 'NONE', #16242, #14117, #3292, .T. ) ;
#17718 = EDGE_LOOP ( 'NONE', ( #15292, #14748, #8219, #17501 ) ) ;
#17719 = ORIENTED_EDGE ( 'NONE', *, *, #6616, .T. ) ;
#17720 = CARTESIAN_POINT ( 'NONE',  ( -85.40000000000000568, -31.83750000000000568, 98.26794919243111792 ) ) ;
#17721 = CARTESIAN_POINT ( 'NONE',  ( -79.39999999999999147, -32.06250000000000000, 101.7320508075688537 ) ) ;
#17722 = CARTESIAN_POINT ( 'NONE',  ( 83.90000000000000568, -32.11874999877097281, -102.5980762113533018 ) ) ;
#17723 = CARTESIAN_POINT ( 'NONE',  ( 83.77821517812500929, -34.11562499938548854, 97.61286128772489690 ) ) ;
#17724 = AXIS2_PLACEMENT_3D ( 'NONE', #16336, #11931, #10657 ) ;
#17725 = CARTESIAN_POINT ( 'NONE',  ( 0.000000000000000000, 3.031088913245532979, -1.750000000000004219 ) ) ;
#17726 = CARTESIAN_POINT ( 'NONE',  ( 235.3564303562499447, -30.40312499938547575, 101.5914258081833879 ) ) ;
#17727 = CARTESIAN_POINT ( 'NONE',  ( 232.5999999999999943, -34.07812499938548001, -46.81714838363331666 ) ) ;
#17728 = CARTESIAN_POINT ( 'NONE',  ( -85.15643035625001289, -35.20312499938548711, 99.99999999999998579 ) ) ;
#17729 = CIRCLE ( 'NONE', #16483, 2.200000000000007283 ) ;
#17730 = CARTESIAN_POINT ( 'NONE',  ( 85.15643035624999868, -34.22812499938547859, 101.5914258081833879 ) ) ;
#17731 = CIRCLE ( 'NONE', #12116, 0.4999999999999978351 ) ;
#17732 = EDGE_CURVE ( 'NONE', #10833, #11539, #11965, .T. ) ;
#17733 = CARTESIAN_POINT ( 'NONE',  ( 81.02178482187500208, -30.44062499938548783, -102.3871387122750889 ) ) ;
#17734 = CARTESIAN_POINT ( 'NONE',  ( 235.5999999999999375, -31.12499999999999645, -50.00000000000011369 ) ) ;
#17735 = EDGE_CURVE ( 'NONE', #11141, #15349, #15334, .T. ) ;
#17736 = CARTESIAN_POINT ( 'NONE',  ( 81.59615242270662350, -34.12634618820329990, 102.9999999999999858 ) ) ;
#17737 = CARTESIAN_POINT ( 'NONE',  ( 81.02178482187500208, -32.69062499938548427, -102.3871387122750889 ) ) ;
#17738 = ORIENTED_EDGE ( 'NONE', *, *, #15919, .F. ) ;
#17739 = DIRECTION ( 'NONE',  ( -1.000000000000000000, -0.000000000000000000, -0.000000000000000000 ) ) ;
#17740 = VECTOR ( 'NONE', #17764, 1000.000000000000000 ) ;
#17741 = CARTESIAN_POINT ( 'NONE',  ( 111.0000000000000000, 10.19999999999997620, -139.9999999999999716 ) ) ;
#17742 = DIRECTION ( 'NONE',  ( -1.000000000000000000, 4.625929269271494788E-16, 0.000000000000000000 ) ) ;
#17743 = CARTESIAN_POINT ( 'NONE',  ( -83.77821517812500929, -33.81562499938548427, 97.61286128772489690 ) ) ;
#17744 = EDGE_LOOP ( 'NONE', ( #16206, #9365, #14742, #14624 ) ) ;
#17745 = CARTESIAN_POINT ( 'NONE',  ( -84.59935209580208948, -35.00000000000002132, 101.7928000422517272 ) ) ;
#17746 = AXIS2_PLACEMENT_3D ( 'NONE', #7073, #19003, #4147 ) ;
#17747 =( BOUNDED_CURVE ( )  B_SPLINE_CURVE ( 2, ( #15992, #14415, #11303, #14225, #18741, #864, #6827, #16089, #8275 ),
 .UNSPECIFIED., .F., .F. ) 
 B_SPLINE_CURVE_WITH_KNOTS ( ( 3, 2, 2, 2, 3 ),
 ( 0.4791666666666666297, 0.4861111111111111049, 0.5000000000000000000, 0.5138888888888888395, 0.5208333333333333703 ),
 .UNSPECIFIED. ) 
 CURVE ( )  GEOMETRIC_REPRESENTATION_ITEM ( )  RATIONAL_B_SPLINE_CURVE ( ( 0.9330127018922194093, 0.9330127018922190762, 1.000000000000000000, 0.8660254037844387076, 1.000000000000000000, 0.8660254037844387076, 1.000000000000000000, 0.9330127018922187432, 0.9330127018922192983 ) ) 
 REPRESENTATION_ITEM ( '' )  );
#17748 = CARTESIAN_POINT ( 'NONE',  ( 231.2217848218749339, -32.46562499938547575, 97.61286128772489690 ) ) ;
#17749 = DIRECTION ( 'NONE',  ( -1.000000000000000000, -0.000000000000000000, -0.000000000000000000 ) ) ;
#17750 = CARTESIAN_POINT ( 'NONE',  ( -83.90000000000000568, -31.87106250001229313, 97.40192378864668399 ) ) ;
#17751 = CARTESIAN_POINT ( 'NONE',  ( 0.3126073911696412022, -2.020725942163688504, 3.500000000000000444 ) ) ;
#17752 = DIRECTION ( 'NONE',  ( 1.000000000000000000, -4.970554372426382520E-17, -0.000000000000000000 ) ) ;
#17753 = CARTESIAN_POINT ( 'NONE',  ( -81.02178482187500208, -31.79062499938548925, 102.3871387122750889 ) ) ;
#17754 = CARTESIAN_POINT ( 'NONE',  ( 230.2491162085250664, -34.99999999999999289, 101.6079878054125487 ) ) ;
#17755 = CARTESIAN_POINT ( 'NONE',  ( 83.77821517812500929, -31.97812499938548925, 97.61286128772489690 ) ) ;
#17756 = CYLINDRICAL_SURFACE ( 'NONE', #18012, 2.649999999999985700 ) ;
#17757 = CARTESIAN_POINT ( 'NONE',  ( -83.77821517812500929, -32.12812499938548427, 97.61286128772489690 ) ) ;
#17758 = CARTESIAN_POINT ( 'NONE',  ( -82.39999999999999147, -30.81562499938548427, -103.1828516163667899 ) ) ;
#17759 = VERTEX_POINT ( 'NONE', #2127 ) ;
#17760 = CARTESIAN_POINT ( 'NONE',  ( 85.40000000000000568, -33.54374999877096286, 99.99999999999998579 ) ) ;
#17761 = FACE_OUTER_BOUND ( 'NONE', #17297, .T. ) ;
#17762 = CARTESIAN_POINT ( 'NONE',  ( 232.5999999999999375, -35.09062499938547575, -46.81714838363331666 ) ) ;
#17763 = CARTESIAN_POINT ( 'NONE',  ( -85.15643035625001289, -30.70312499938548711, 99.99999999999998579 ) ) ;
#17764 = DIRECTION ( 'NONE',  ( 1.387778780781445676E-15, 1.000000000000000000, 0.000000000000000000 ) ) ;
#17765 = ORIENTED_EDGE ( 'NONE', *, *, #6731, .F. ) ;
#17766 = CARTESIAN_POINT ( 'NONE',  ( -79.64356964374999848, -34.86562499938548143, -99.99999999999998579 ) ) ;
#17767 = CARTESIAN_POINT ( 'NONE',  ( 4.203935335434060505, 1.640780671294165272, -3.598452447879202598 ) ) ;
#17768 = VERTEX_POINT ( 'NONE', #13838 ) ;
#17769 = CARTESIAN_POINT ( 'NONE',  ( 229.5999999999999375, -33.60000000000000142, -50.00000000000011369 ) ) ;
#17770 = EDGE_CURVE ( 'NONE', #17953, #198, #3485, .T. ) ;
#17771 = CARTESIAN_POINT ( 'NONE',  ( -81.02178482187500208, -33.10312499938548569, -102.3871387122750889 ) ) ;
#17772 = CARTESIAN_POINT ( 'NONE',  ( -79.79868554276779946, -32.00000000000000711, -101.4716133421136846 ) ) ;
#17773 = CARTESIAN_POINT ( 'NONE',  ( -79.39999999999999147, -32.45624999877097139, -98.26794919243113213 ) ) ;
#17774 = CARTESIAN_POINT ( 'NONE',  ( 235.3564303562499447, -32.76562499938548001, 101.5914258081833879 ) ) ;
#17775 = CARTESIAN_POINT ( 'NONE',  ( -79.39999999999999147, -32.38518749875867542, 98.26794919243110371 ) ) ;
#17776 = CARTESIAN_POINT ( 'NONE',  ( -83.77821517812500929, -33.77812499938548285, 102.3871387122750889 ) ) ;
#17777 = CARTESIAN_POINT ( 'NONE',  ( -81.02178482187500208, -34.04062499938548569, -97.61286128772489690 ) ) ;
#17778 = DIRECTION ( 'NONE',  ( -1.000000000000000000, 0.000000000000000000, 0.000000000000000000 ) ) ;
#17779 = DIRECTION ( 'NONE',  ( 0.000000000000000000, 0.000000000000000000, -1.000000000000000000 ) ) ;
#17780 = CARTESIAN_POINT ( 'NONE',  ( 79.39999999999999147, -32.38124999877096855, -98.26794919243110371 ) ) ;
#17781 = CARTESIAN_POINT ( 'NONE',  ( 235.5999999999999943, -33.41250000000000142, 101.7320508075688537 ) ) ;
#17782 = PRODUCT_RELATED_PRODUCT_CATEGORY ( 'part', '', ( #10904 ) ) ;
#17783 = ORIENTED_EDGE ( 'NONE', *, *, #9772, .T. ) ;
#17784 = CARTESIAN_POINT ( 'NONE',  ( 105.1999999999999602, -29.80000000000001492, -97.80000000000002558 ) ) ;
#17785 = CARTESIAN_POINT ( 'NONE',  ( 230.3018604581529871, -35.39427337414328889, 98.07164457472185859 ) ) ;
#17786 = CARTESIAN_POINT ( 'NONE',  ( 232.5999999999999375, -32.30624999877095860, -53.46410161513786363 ) ) ;
#17787 = CARTESIAN_POINT ( 'NONE',  ( -83.77821517812500929, -33.21562499938548285, 102.3871387122750889 ) ) ;
#17788 = VERTEX_POINT ( 'NONE', #15411 ) ;
#17789 = VERTEX_POINT ( 'NONE', #7793 ) ;
#17790 = CARTESIAN_POINT ( 'NONE',  ( 79.39999999999999147, -34.31250000000000000, -101.7320508075688537 ) ) ;
#17791 = CARTESIAN_POINT ( 'NONE',  ( -4.000000000000000000, -2.472261339043343220, -3.687027428081192326 ) ) ;
#17792 = CARTESIAN_POINT ( 'NONE',  ( -82.40000000000000568, -32.30624999877097281, 97.00000000000000000 ) ) ;
#17793 = ORIENTED_EDGE ( 'NONE', *, *, #11611, .T. ) ;
#17794 = CARTESIAN_POINT ( 'NONE',  ( -79.83361526238435601, -35.00000000000000711, 101.0217260113603572 ) ) ;
#17795 = CARTESIAN_POINT ( 'NONE',  ( -83.77821517812500929, -33.02812499938548285, 97.61286128772489690 ) ) ;
#17796 = CARTESIAN_POINT ( 'NONE',  ( -82.39999999999999147, -33.03750000000000142, 103.4641016151377499 ) ) ;
#17797 = CARTESIAN_POINT ( 'NONE',  ( -85.40000000000000568, -31.74374999877096926, 99.99999999999998579 ) ) ;
#17798 = PLANE ( 'NONE',  #8808 ) ;
#17799 = CARTESIAN_POINT ( 'NONE',  ( -82.41196654184768988, -35.00000000000000711, -102.9991646027828693 ) ) ;
#17800 = CARTESIAN_POINT ( 'NONE',  ( 235.3564303562499447, -30.32812499938548001, 98.40857419181659793 ) ) ;
#17801 = ORIENTED_EDGE ( 'NONE', *, *, #17357, .F. ) ;
#17802 = ADVANCED_FACE ( 'NONE', ( #2021 ), #6431, .T. ) ;
#17803 = FILL_AREA_STYLE_COLOUR ( '', #6802 ) ;
#17804 = CARTESIAN_POINT ( 'NONE',  ( -83.77821517812500929, -31.11562499938548498, -102.3871387122750889 ) ) ;
#17805 = CARTESIAN_POINT ( 'NONE',  ( -83.20384757729337366, -33.50759618943233420, 103.0000000000000000 ) ) ;
#17806 = CARTESIAN_POINT ( 'NONE',  ( 244.7999999999999545, -4.999999999999976907, 153.0000000000000000 ) ) ;
#17807 = LINE ( 'NONE', #12031, #7102 ) ;
#17808 = CARTESIAN_POINT ( 'NONE',  ( -79.64356964375001269, -32.12812499938548427, 98.40857419181659793 ) ) ;
#17809 = CARTESIAN_POINT ( 'NONE',  ( 82.39999999999999147, -34.33124999877097139, 97.00000000000000000 ) ) ;
#17810 = CARTESIAN_POINT ( 'NONE',  ( 235.3564303562499447, -32.65312499938547575, -48.40857419181671162 ) ) ;
#17811 = EDGE_LOOP ( 'NONE', ( #4254, #15840, #5024, #1085 ) ) ;
#17812 = ORIENTED_EDGE ( 'NONE', *, *, #4882, .F. ) ;
#17813 = CARTESIAN_POINT ( 'NONE',  ( -83.20384757729337366, -31.70759618943234059, 103.0000000000000000 ) ) ;
#17814 = CARTESIAN_POINT ( 'NONE',  ( -83.88339518848731302, -35.16733441503058089, 97.47959136244114120 ) ) ;
#17815 = CARTESIAN_POINT ( 'NONE',  ( -79.39999999999999147, -32.38124999877096855, 98.26794919243110371 ) ) ;
#17816 = CARTESIAN_POINT ( 'NONE',  ( 83.90000000000000568, -33.07500000000000284, 97.40192378864668399 ) ) ;
#17817 = CARTESIAN_POINT ( 'NONE',  ( -82.86160995759659897, -32.00000000000002132, -97.18959324165045643 ) ) ;
#17818 = CARTESIAN_POINT ( 'NONE',  ( 235.3564303562499447, -34.00312499938547717, 101.5914258081833879 ) ) ;
#17819 = CARTESIAN_POINT ( 'NONE',  ( 85.40000000000000568, -32.15624999877096712, 98.26794919243111792 ) ) ;
#17820 = CARTESIAN_POINT ( 'NONE',  ( 79.64356964375001269, -33.47812499938547859, 101.5914258081833879 ) ) ;
#17821 = EDGE_CURVE ( 'NONE', #10754, #16690, #13747, .T. ) ;
#17822 = CARTESIAN_POINT ( 'NONE',  ( 79.64356964375001269, -30.40312499938548285, -101.5914258081833879 ) ) ;
#17823 = CARTESIAN_POINT ( 'NONE',  ( 229.8435696437499871, -35.05312499938547433, -48.40857419181671162 ) ) ;
#17824 = CARTESIAN_POINT ( 'NONE',  ( -82.39999999999999147, -34.75312499938548427, 96.81714838363319586 ) ) ;
#17825 = CARTESIAN_POINT ( 'NONE',  ( 82.39999999999999147, -34.07812499938548711, -103.1828516163667899 ) ) ;
#17826 = ORIENTED_EDGE ( 'NONE', *, *, #2937, .T. ) ;
#17827 = DIRECTION ( 'NONE',  ( 0.000000000000000000, 0.000000000000000000, 1.000000000000000000 ) ) ;
#17828 = CYLINDRICAL_SURFACE ( 'NONE', #3363, 2.649999999999985700 ) ;
#17829 = CARTESIAN_POINT ( 'NONE',  ( 229.8435696437499303, -31.60312499938548214, -50.00000000000011369 ) ) ;
#17830 = CARTESIAN_POINT ( 'NONE',  ( -83.90000000000000568, -31.42500000000000071, 97.40192378864668399 ) ) ;
#17831 = ORIENTED_EDGE ( 'NONE', *, *, #12813, .T. ) ;
#17832 = CARTESIAN_POINT ( 'NONE',  ( -69.99999999999998579, -35.00000000000000000, 150.0000000000000000 ) ) ;
#17833 = EDGE_CURVE ( 'NONE', #17788, #198, #15120, .T. ) ;
#17834 = CARTESIAN_POINT ( 'NONE',  ( -80.90000000000000568, -30.99374999877096926, 97.40192378864668399 ) ) ;
#17835 = CARTESIAN_POINT ( 'NONE',  ( -82.39999999999999147, -34.33124999877097139, -97.00000000000000000 ) ) ;
#17836 = CARTESIAN_POINT ( 'NONE',  ( -80.90000000000000568, -33.44606250001229597, 102.5980762113533018 ) ) ;
#17837 = DIRECTION ( 'NONE',  ( 1.000000000000000000, 0.000000000000000000, -0.000000000000000000 ) ) ;
#17838 = CARTESIAN_POINT ( 'NONE',  ( 230.8769377533405986, -32.00000000000000711, -47.80849716182774500 ) ) ;
#17839 = CARTESIAN_POINT ( 'NONE',  ( -81.02178482187500208, -30.89062499938548711, 102.3871387122750889 ) ) ;
#17840 = DIRECTION ( 'NONE',  ( -1.000000000000000000, -0.000000000000000000, 0.000000000000000000 ) ) ;
#17841 = CARTESIAN_POINT ( 'NONE',  ( 83.77821517812500929, -31.67812499938548498, 102.3871387122750889 ) ) ;
#17842 = EDGE_CURVE ( 'NONE', #13089, #893, #11005, .T. ) ;
#17843 = CARTESIAN_POINT ( 'NONE',  ( 25.60000000000000142, 2.789133085058097101E-16, -2.055000000000000160 ) ) ;
#17844 = CARTESIAN_POINT ( 'NONE',  ( 231.0999999999999375, -34.81874999877096144, 102.5980762113533018 ) ) ;
#17845 = B_SPLINE_CURVE_WITH_KNOTS ( 'NONE', 3,
 ( #17095, #2047, #14156, #8006, #8207, #15536, #4997, #790, #411, #2152, #12692, #3707, #8109, #9673, #3419, #9371, #11229, #18666 ),
 .UNSPECIFIED., .F., .F.,
 ( 4, 2, 2, 2, 2, 2, 2, 2, 4 ),
 ( 0.000000000000000000, 0.0007089252359871620014, 0.001417850471974324003, 0.002126775707961485896, 0.002835700943948648006, 0.003544626179935810115, 0.004253551415922971791, 0.004962476651910133901, 0.005671401887897296011 ),
 .UNSPECIFIED. ) ;
#17846 = CARTESIAN_POINT ( 'NONE',  ( 84.51155386534844638, -35.25364837475780888, -98.22820752270799005 ) ) ;
#17847 = CARTESIAN_POINT ( 'NONE',  ( -85.15643035624999868, -32.01562499938548711, -98.40857419181659793 ) ) ;
#17848 = ORIENTED_EDGE ( 'NONE', *, *, #15121, .T. ) ;
#17849 = CARTESIAN_POINT ( 'NONE',  ( 79.64356964374999848, -30.92812499938548498, 99.99999999999998579 ) ) ;
#17850 = CARTESIAN_POINT ( 'NONE',  ( 83.90000000000000568, -34.36874999877097281, 97.40192378864668399 ) ) ;
#17851 = CARTESIAN_POINT ( 'NONE',  ( 235.3564303562499447, -34.94062499938547717, -51.59142580818350865 ) ) ;
#17852 = CIRCLE ( 'NONE', #389, 2.200000000000007283 ) ;
#17853 =( BOUNDED_SURFACE ( )  B_SPLINE_SURFACE ( 3, 2, ( 
 ( #2940, #1480, #9990 ),
 ( #1093, #4606, #25 ),
 ( #15338, #10562, #12124 ),
 ( #16712, #219, #17897 ),
 ( #10842, #3319, #9280 ),
 ( #1860, #13579, #1954 ) ),
 .UNSPECIFIED., .F., .F., .T. ) 
 B_SPLINE_SURFACE_WITH_KNOTS ( ( 4, 2, 4 ),
 ( 3, 3 ),
 ( 0.01651999345535505245, 0.01858032176739834659, 0.02064065007944164074 ),
 ( 0.000000000000000000, 1.000000000000000000 ),
 .UNSPECIFIED. ) 
 GEOMETRIC_REPRESENTATION_ITEM ( )  RATIONAL_B_SPLINE_SURFACE ( (
 ( 1.000000000000000000, 0.8047781103519393575, 1.000000000000000000),
 ( 1.000000000000000000, 0.8123785825605439603, 1.000000000000000000),
 ( 1.000000000000000000, 0.8190671539786830158, 1.000000000000000000),
 ( 1.000000000000000000, 0.8192352254836331449, 1.000000000000000000),
 ( 1.000000000000000000, 0.8126129677210507385, 1.000000000000000000),
 ( 1.000000000000000000, 0.8047712537969728963, 1.000000000000000000) ) ) 
 REPRESENTATION_ITEM ( '' )  SURFACE ( )  );
#17854 = VECTOR ( 'NONE', #10378, 1000.000000000000000 ) ;
#17855 = CARTESIAN_POINT ( 'NONE',  ( -79.64356964375001269, -32.24062499938548854, 98.40857419181659793 ) ) ;
#17856 = CYLINDRICAL_SURFACE ( 'NONE', #9618, 3.000000000000002665 ) ;
#17857 = EDGE_LOOP ( 'NONE', ( #18023, #1615, #14993, #2600 ) ) ;
#17858 = CARTESIAN_POINT ( 'NONE',  ( -79.64356964375001269, -33.55312499938548854, -98.40857419181659793 ) ) ;
#17859 = CARTESIAN_POINT ( 'NONE',  ( 80.90000000000000568, -32.49374999877097281, 97.40192378864668399 ) ) ;
#17860 = ADVANCED_FACE ( 'NONE', ( #3585 ), #6242, .T. ) ;
#17861 = CARTESIAN_POINT ( 'NONE',  ( 231.7961524227065979, -33.50759618943233420, -47.00000000000011369 ) ) ;
#17862 = CARTESIAN_POINT ( 'NONE',  ( -83.77821517812500929, -33.92812499938548854, -102.3871387122750889 ) ) ;
#17863 = CARTESIAN_POINT ( 'NONE',  ( 229.5999999999999375, -33.50624999877096144, -48.26794919243123161 ) ) ;
#17864 = CARTESIAN_POINT ( 'NONE',  ( -85.40000000000000568, -31.74374999877096926, -99.99999999999998579 ) ) ;
#17865 = CARTESIAN_POINT ( 'NONE',  ( 235.3564303562499447, -31.37812499938547717, 99.99999999999998579 ) ) ;
#17866 = CARTESIAN_POINT ( 'NONE',  ( -80.90000000000000568, -31.44768749875867542, 97.40192378864668399 ) ) ;
#17867 = CARTESIAN_POINT ( 'NONE',  ( -85.15643035625001289, -33.85312499938549280, 99.99999999999998579 ) ) ;
#17868 = DIRECTION ( 'NONE',  ( -0.000000000000000000, -1.000000000000000000, -0.000000000000000000 ) ) ;
#17869 = CARTESIAN_POINT ( 'NONE',  ( 85.15643035625001289, -33.32812499938548711, 101.5914258081833879 ) ) ;
#17870 = CARTESIAN_POINT ( 'NONE',  ( 79.39999999999999147, -32.51250000000000284, -101.7320508075688537 ) ) ;
#17871 =( GEOMETRIC_REPRESENTATION_CONTEXT ( 3 ) GLOBAL_UNCERTAINTY_ASSIGNED_CONTEXT ( ( #15785 ) ) GLOBAL_UNIT_ASSIGNED_CONTEXT ( ( #16137, #9988, #15943 ) ) REPRESENTATION_CONTEXT ( 'NONE', 'WORKASPACE' ) );
#17872 = MECHANICAL_DESIGN_GEOMETRIC_PRESENTATION_REPRESENTATION (  '', ( #6011 ), #11629 ) ;
#17873 = CARTESIAN_POINT ( 'NONE',  ( 235.5999999999999943, -33.35624999877096286, 101.7320508075688537 ) ) ;
#17874 = CARTESIAN_POINT ( 'NONE',  ( 83.90000000000000568, -34.81874999877096855, -102.5980762113533018 ) ) ;
#17875 = CARTESIAN_POINT ( 'NONE',  ( 235.5999999999999943, -33.86249999999999716, 101.7320508075688537 ) ) ;
#17876 = ORIENTED_EDGE ( 'NONE', *, *, #12122, .T. ) ;
#17877 = CARTESIAN_POINT ( 'NONE',  ( 233.9782151781249411, -33.10312499938547859, -52.38713871227520968 ) ) ;
#17878 = CARTESIAN_POINT ( 'NONE',  ( 91.99999999999994316, -21.80000000000002913, -140.0000000000000000 ) ) ;
#17879 = ADVANCED_FACE ( 'NONE', ( #4678 ), #12290, .F. ) ;
#17880 = CARTESIAN_POINT ( 'NONE',  ( 229.5999999999999943, -35.36739044046695568, 98.90809476984486537 ) ) ;
#17881 = CARTESIAN_POINT ( 'NONE',  ( 229.5999999999999375, -33.58124999877096428, -51.73205080756898866 ) ) ;
#17882 = CARTESIAN_POINT ( 'NONE',  ( -83.77821517812500929, -34.56562499938548427, 102.3871387122750889 ) ) ;
#17883 = ORIENTED_EDGE ( 'NONE', *, *, #3514, .T. ) ;
#17884 = VERTEX_POINT ( 'NONE', #16593 ) ;
#17885 = CARTESIAN_POINT ( 'NONE',  ( -80.90000000000000568, -32.10000000000000142, 102.5980762113533018 ) ) ;
#17886 = AXIS2_PLACEMENT_3D ( 'NONE', #16918, #15449, #3233 ) ;
#17887 = CARTESIAN_POINT ( 'NONE',  ( -4.197477534772231955, 0.8522413273724368521, -3.505042416683225692 ) ) ;
#17888 = DIRECTION ( 'NONE',  ( -0.000000000000000000, -1.000000000000000000, -0.000000000000000000 ) ) ;
#17889 = VERTEX_POINT ( 'NONE', #3198 ) ;
#17890 = DIRECTION ( 'NONE',  ( 0.000000000000000000, 6.982962677686266711E-15, -1.000000000000000000 ) ) ;
#17891 = DIRECTION ( 'NONE',  ( 4.625929269271494788E-16, 1.000000000000000000, -0.000000000000000000 ) ) ;
#17892 = CARTESIAN_POINT ( 'NONE',  ( -81.02178482187500208, -35.05312499938548854, 102.3871387122750889 ) ) ;
#17893 = CARTESIAN_POINT ( 'NONE',  ( -85.40000000000000568, -34.08749999999999858, 98.26794919243111792 ) ) ;
#17894 = CARTESIAN_POINT ( 'NONE',  ( -85.40000000000000568, -31.78124999877096712, 98.26794919243111792 ) ) ;
#17895 = DIRECTION ( 'NONE',  ( 0.000000000000000000, 0.000000000000000000, -1.000000000000000000 ) ) ;
#17896 =( NAMED_UNIT ( * ) PLANE_ANGLE_UNIT ( ) SI_UNIT ( $, .RADIAN. ) );
#17897 = CARTESIAN_POINT ( 'NONE',  ( 3.972066048304702779, 3.435565134476335380, 1.180968096049678229 ) ) ;
#17898 = DIRECTION ( 'NONE',  ( -0.000000000000000000, -1.000000000000000000, -0.000000000000000000 ) ) ;
#17899 = DIRECTION ( 'NONE',  ( -1.000000000000000000, 0.000000000000000000, 0.000000000000000000 ) ) ;
#17900 = ORIENTED_EDGE ( 'NONE', *, *, #15807, .F. ) ;
#17901 =( LENGTH_UNIT ( ) NAMED_UNIT ( * ) SI_UNIT ( .MILLI., .METRE. ) );
#17902 = CARTESIAN_POINT ( 'NONE',  ( -79.64356964375001269, -32.12812499938548427, -101.5914258081833879 ) ) ;
#17903 = FACE_OUTER_BOUND ( 'NONE', #16830, .T. ) ;
#17904 = CARTESIAN_POINT ( 'NONE',  ( 0.3126073911696428675, 4.041451884327382338, -3.240528425403984455E-16 ) ) ;
#17905 =( BOUNDED_CURVE ( )  B_SPLINE_CURVE ( 2, ( #7902, #4989, #6162, #9268, #6258, #10832, #16802, #15235, #3412 ),
 .UNSPECIFIED., .F., .F. ) 
 B_SPLINE_CURVE_WITH_KNOTS ( ( 3, 2, 2, 2, 3 ),
 ( 0.7291666666666668517, 0.7361111111111111605, 0.7500000000000000000, 0.7638888888888888395, 0.7708333333333332593 ),
 .UNSPECIFIED. ) 
 CURVE ( )  GEOMETRIC_REPRESENTATION_ITEM ( )  RATIONAL_B_SPLINE_CURVE ( ( 0.9330127018922194093, 0.9330127018922209636, 1.000000000000000000, 0.8660254037844387076, 1.000000000000000000, 0.8660254037844387076, 1.000000000000000000, 0.9330127018922198534, 0.9330127018922192983 ) ) 
 REPRESENTATION_ITEM ( '' )  );
#17906 = CARTESIAN_POINT ( 'NONE',  ( 80.17984880387895430, -35.00000000000000000, -101.6434491389460817 ) ) ;
#17907 = CARTESIAN_POINT ( 'NONE',  ( -83.77821517812500929, -31.41562499938548569, 102.3871387122750889 ) ) ;
#17908 = DIRECTION ( 'NONE',  ( 1.000000000000000000, 0.000000000000000000, 0.000000000000000000 ) ) ;
#17909 = CARTESIAN_POINT ( 'NONE',  ( 232.5999999999999375, -33.17812499938548143, -46.81714838363331666 ) ) ;
#17910 = ORIENTED_EDGE ( 'NONE', *, *, #16871, .F. ) ;
#17911 = ORIENTED_EDGE ( 'NONE', *, *, #15817, .F. ) ;
#17912 = CYLINDRICAL_SURFACE ( 'NONE', #3840, 3.000000000000009770 ) ;
#17913 = CARTESIAN_POINT ( 'NONE',  ( -85.40000000000000568, -30.41249999999999787, 101.7320508075688679 ) ) ;
#17914 = CARTESIAN_POINT ( 'NONE',  ( -85.40000000000000568, -32.68124999877097281, 98.26794919243111792 ) ) ;
#17915 = CARTESIAN_POINT ( 'NONE',  ( 83.90000000000000568, -31.27500000000000568, 97.40192378864668399 ) ) ;
#17916 = CARTESIAN_POINT ( 'NONE',  ( 82.40000000000001990, -32.53124999877097423, 97.00000000000000000 ) ) ;
#17917 = CARTESIAN_POINT ( 'NONE',  ( 231.2217848218749339, -33.66562499938547859, 102.3871387122750889 ) ) ;
#17918 = CARTESIAN_POINT ( 'NONE',  ( 229.8435696437499587, -34.60312499938547859, -48.40857419181671162 ) ) ;
#17919 = CARTESIAN_POINT ( 'NONE',  ( 82.39999999999999147, -34.07812499938548711, 96.81714838363319586 ) ) ;
#17920 = CARTESIAN_POINT ( 'NONE',  ( 79.64356964375001269, -32.20312499938548001, -101.5914258081833879 ) ) ;
#17921 = ORIENTED_EDGE ( 'NONE', *, *, #9148, .T. ) ;
#17922 = CARTESIAN_POINT ( 'NONE',  ( 229.5999999999999375, -30.48749999999999005, -51.73205080756898866 ) ) ;
#17923 = CARTESIAN_POINT ( 'NONE',  ( 81.59615242270662350, -34.31115380933863435, 96.99999999999998579 ) ) ;
#17924 = CARTESIAN_POINT ( 'NONE',  ( 85.15643035624999868, -32.87812499938549138, -98.40857419181659793 ) ) ;
#17925 = DIRECTION ( 'NONE',  ( -1.000000000000000000, 0.000000000000000000, 0.000000000000000000 ) ) ;
#17926 = DIRECTION ( 'NONE',  ( 0.000000000000000000, 0.000000000000000000, -1.000000000000000000 ) ) ;
#17927 = CARTESIAN_POINT ( 'NONE',  ( 233.9782151781249411, -30.40312499938547930, -52.38713871227520968 ) ) ;
#17928 = CARTESIAN_POINT ( 'NONE',  ( -85.40000000000000568, -30.86250000000000071, 101.7320508075688679 ) ) ;
#17929 = VERTEX_POINT ( 'NONE', #9157 ) ;
#17930 = DIRECTION ( 'NONE',  ( 0.8191520442889902442, 1.003171929053522651E-16, -0.5735764363510482688 ) ) ;
#17932 = CARTESIAN_POINT ( 'NONE',  ( -79.39999999999999147, -34.27499999999999858, 99.99999999999998579 ) ) ;
#17931 =( BOUNDED_CURVE ( )  B_SPLINE_CURVE ( 2, ( #10691, #18319, #16658, #7475, #11962, #9127, #3260, #1897, #4745 ),
 .UNSPECIFIED., .F., .F. ) 
 B_SPLINE_CURVE_WITH_KNOTS ( ( 3, 2, 2, 2, 3 ),
 ( 0.4375000000000000555, 0.4444444444444444198, 0.4583333333333333148, 0.4722222222222222099, 0.4791666666666666297 ),
 .UNSPECIFIED. ) 
 CURVE ( )  GEOMETRIC_REPRESENTATION_ITEM ( )  RATIONAL_B_SPLINE_CURVE ( ( 0.9330127018922192983, 0.9330127018922198534, 1.000000000000000000, 0.8660254037844387076, 1.000000000000000000, 0.8660254037844387076, 1.000000000000000000, 0.9330127018922196314, 0.9330127018922194093 ) ) 
 REPRESENTATION_ITEM ( '' )  );
#17933 = CARTESIAN_POINT ( 'NONE',  ( 85.15643035624999868, -30.62812499938548427, 101.5914258081833879 ) ) ;
#17934 = CARTESIAN_POINT ( 'NONE',  ( -79.39999999999999147, -31.98356250001229384, 98.26794919243110371 ) ) ;
#17935 = CARTESIAN_POINT ( 'NONE',  ( -4.000000000000000000, 2.309401076758498483, -3.433295621305379353 ) ) ;
#17936 = CARTESIAN_POINT ( 'NONE',  ( -82.40000000000000568, -32.08124999877097139, 102.9999999999999858 ) ) ;
#17937 = CARTESIAN_POINT ( 'NONE',  ( -82.39999999999999147, -32.05312499938548854, 96.81714838363319586 ) ) ;
#17938 = CARTESIAN_POINT ( 'NONE',  ( 244.7999999999999545, -4.999999999999976907, 150.0000000000000000 ) ) ;
#17939 = CARTESIAN_POINT ( 'NONE',  ( 81.02178482187500208, -33.10312499938548569, 102.3871387122750889 ) ) ;
#17940 = CARTESIAN_POINT ( 'NONE',  ( 82.39999999999999147, -30.36562499938549209, -96.81714838363319586 ) ) ;
#17941 = FACE_OUTER_BOUND ( 'NONE', #3554, .T. ) ;
#17942 = CARTESIAN_POINT ( 'NONE',  ( 85.15643035625001289, -35.22676544108147567, -98.99674642581742035 ) ) ;
#17943 = CARTESIAN_POINT ( 'NONE',  ( -81.02178482187500208, -31.45312499938549067, -97.61286128772489690 ) ) ;
#17944 = ORIENTED_EDGE ( 'NONE', *, *, #13225, .T. ) ;
#17945 = CARTESIAN_POINT ( 'NONE',  ( 79.64356964375001269, -30.44062499938548783, 101.5914258081833879 ) ) ;
#17946 = DIRECTION ( 'NONE',  ( -0.000000000000000000, -0.000000000000000000, -1.000000000000000000 ) ) ;
#17947 = CARTESIAN_POINT ( 'NONE',  ( 83.20384757729337366, -32.55134618820330417, 97.00000000000000000 ) ) ;
#17948 = EDGE_CURVE ( 'NONE', #8464, #8905, #12189, .T. ) ;
#17949 = VECTOR ( 'NONE', #9643, 1000.000000000000000 ) ;
#17950 = CARTESIAN_POINT ( 'NONE',  ( -85.40000000000000568, -33.14999999999999858, 99.99999999999998579 ) ) ;
#17951 = CARTESIAN_POINT ( 'NONE',  ( -83.77821517812500929, -32.42812499938548854, 102.3871387122750889 ) ) ;
#17952 = CARTESIAN_POINT ( 'NONE',  ( 244.7999999999999545, -29.80000000000000426, -100.0000000000000000 ) ) ;
#17953 = VERTEX_POINT ( 'NONE', #10816 ) ;
#17954 = CARTESIAN_POINT ( 'NONE',  ( -82.39999999999999147, -31.68750000000000355, -96.53589838486223584 ) ) ;
#17955 = FACE_OUTER_BOUND ( 'NONE', #18676, .T. ) ;
#17956 = ADVANCED_FACE ( 'NONE', ( #16783 ), #16806, .T. ) ;
#17957 = CARTESIAN_POINT ( 'NONE',  ( -85.40000000000000568, -34.93124999877096570, -101.7320508075688821 ) ) ;
#17958 = CARTESIAN_POINT ( 'NONE',  ( -85.15643035624999868, -32.91562499938549280, -98.40857419181659793 ) ) ;
#17959 = CARTESIAN_POINT ( 'NONE',  ( 231.0999999999999375, -33.46874999877096002, -47.40192378864679768 ) ) ;
#17960 = CARTESIAN_POINT ( 'NONE',  ( 232.5999999999999375, -32.16562499938547859, 96.81714838363319586 ) ) ;
#17961 = CARTESIAN_POINT ( 'NONE',  ( -80.90000000000000568, -32.34768749875867400, 97.40192378864668399 ) ) ;
#17962 = CARTESIAN_POINT ( 'NONE',  ( -83.77821517812500929, -34.67812499938548854, 102.3871387122750889 ) ) ;
#17963 = CARTESIAN_POINT ( 'NONE',  ( -81.02178482187500208, -34.49062499938548854, -97.61286128772489690 ) ) ;
#17964 = CARTESIAN_POINT ( 'NONE',  ( 83.77821517812500929, -33.81562499938548427, 102.3871387122750889 ) ) ;
#17965 = CYLINDRICAL_SURFACE ( 'NONE', #3999, 10.00000000000000000 ) ;
#17966 = AXIS2_PLACEMENT_3D ( 'NONE', #8746, #10406, #12065 ) ;
#17967 = DIRECTION ( 'NONE',  ( -1.000000000000000000, 1.586032892321652285E-15, -0.000000000000000000 ) ) ;
#17968 = CARTESIAN_POINT ( 'NONE',  ( 83.90000000000000568, -34.36874999877097281, -102.5980762113533018 ) ) ;
#17969 = CARTESIAN_POINT ( 'NONE',  ( 235.5999999999999375, -33.37499999999999289, 99.99999999999998579 ) ) ;
#17970 =( BOUNDED_CURVE ( )  B_SPLINE_CURVE ( 2, ( #17195, #606, #12312, #15437, #6652, #12598, #18567, #3610, #6555 ),
 .UNSPECIFIED., .F., .F. ) 
 B_SPLINE_CURVE_WITH_KNOTS ( ( 3, 2, 2, 2, 3 ),
 ( 0.6875000000000000000, 0.6944444444444444198, 0.7083333333333333703, 0.7222222222222222099, 0.7291666666666666297 ),
 .UNSPECIFIED. ) 
 CURVE ( )  GEOMETRIC_REPRESENTATION_ITEM ( )  RATIONAL_B_SPLINE_CURVE ( ( 0.9330127018922194093, 0.9330127018922194093, 1.000000000000000000, 0.8660254037844387076, 1.000000000000000000, 0.8660254037844387076, 1.000000000000000000, 0.9330127018922198534, 0.9330127018922192983 ) ) 
 REPRESENTATION_ITEM ( '' )  );
#17971 = EDGE_CURVE ( 'NONE', #8657, #12671, #17456, .T. ) ;
#17972 = ORIENTED_EDGE ( 'NONE', *, *, #11143, .F. ) ;
#17973 = CARTESIAN_POINT ( 'NONE',  ( 232.5999999999999943, -33.96562499938547575, -53.18285161636690361 ) ) ;
#17974 = DIRECTION ( 'NONE',  ( 0.000000000000000000, 0.000000000000000000, 1.000000000000000000 ) ) ;
#17975 = CARTESIAN_POINT ( 'NONE',  ( 232.5999999999999375, -34.10624999877096286, 96.53589838486223584 ) ) ;
#17976 = CARTESIAN_POINT ( 'NONE',  ( 235.5999999999999943, -32.38124999877096144, -51.73205080756900287 ) ) ;
#17977 = EDGE_CURVE ( 'NONE', #11363, #9248, #5550, .T. ) ;
#17978 = CARTESIAN_POINT ( 'NONE',  ( -83.77821517812500929, -32.46562499938548285, 97.61286128772489690 ) ) ;
#17979 = ORIENTED_EDGE ( 'NONE', *, *, #1374, .F. ) ;
#17980 = ORIENTED_EDGE ( 'NONE', *, *, #10096, .F. ) ;
#17981 = CARTESIAN_POINT ( 'NONE',  ( 229.5999999999999375, -32.64374999877096428, -50.00000000000011369 ) ) ;
#17982 = AXIS2_PLACEMENT_3D ( 'NONE', #18043, #17840, #6218 ) ;
#17983 = CARTESIAN_POINT ( 'NONE',  ( -4.000000000000000000, -1.680117682357936904, -3.316611593218794951 ) ) ;
#17984 = DIRECTION ( 'NONE',  ( 0.000000000000000000, 0.000000000000000000, 1.000000000000000000 ) ) ;
#17985 = EDGE_LOOP ( 'NONE', ( #16068, #12513, #15469, #15568 ) ) ;
#17986 = FACE_OUTER_BOUND ( 'NONE', #15063, .T. ) ;
#17987 = CARTESIAN_POINT ( 'NONE',  ( -82.39999999999999147, -33.20624999877097849, -103.0000000000000000 ) ) ;
#17988 = CARTESIAN_POINT ( 'NONE',  ( -81.02178482187500208, -34.60312499938549280, 102.3871387122750889 ) ) ;
#17989 = CARTESIAN_POINT ( 'NONE',  ( -85.40000000000000568, -33.60000000000000142, 99.99999999999998579 ) ) ;
#17990 = CARTESIAN_POINT ( 'NONE',  ( -79.39999999999999147, -31.06874999877096855, 99.99999999999998579 ) ) ;
#17991 = CARTESIAN_POINT ( 'NONE',  ( 235.4117376914898898, -32.00000000000000000, -51.04600724388262023 ) ) ;
#17992 = STYLED_ITEM ( 'NONE', ( #4009 ), #10882 ) ;
#17993 = CARTESIAN_POINT ( 'NONE',  ( 235.5999999999999943, -33.33749999999999147, 98.26794919243110371 ) ) ;
#17994 = CYLINDRICAL_SURFACE ( 'NONE', #12115, 3.000000000000002665 ) ;
#17995 = CARTESIAN_POINT ( 'NONE',  ( -82.40000000000000568, -30.00000000000000355, 99.99999999999998579 ) ) ;
#17996 = VECTOR ( 'NONE', #8956, 1000.000000000000000 ) ;
#17997 = CARTESIAN_POINT ( 'NONE',  ( -85.40000000000000568, -34.44374999877096855, -99.99999999999998579 ) ) ;
#17998 = EDGE_LOOP ( 'NONE', ( #13969, #13850, #13918, #18572 ) ) ;
#17999 =( LENGTH_UNIT ( ) NAMED_UNIT ( * ) SI_UNIT ( .MILLI., .METRE. ) );
#18000 = CARTESIAN_POINT ( 'NONE',  ( -79.64356964375001269, -33.92812499938548854, -101.5914258081833879 ) ) ;
#18001 = CARTESIAN_POINT ( 'NONE',  ( 3.349226789952652439, 2.685125164760731487, -0.2236248678334773199 ) ) ;
#18002 = CARTESIAN_POINT ( 'NONE',  ( 231.0999999999999375, -34.36874999877096570, 102.5980762113533018 ) ) ;
#18003 = CARTESIAN_POINT ( 'NONE',  ( -85.15643035624999868, -30.62812499938548427, 98.40857419181659793 ) ) ;
#18004 = CARTESIAN_POINT ( 'NONE',  ( -82.40000000000000568, -33.43124999877096570, 102.9999999999999858 ) ) ;
#18005 = EDGE_CURVE ( 'NONE', #11737, #17562, #16735, .T. ) ;
#18006 = CARTESIAN_POINT ( 'NONE',  ( 231.2217848218749339, -32.46562499938547575, -52.38713871227520968 ) ) ;
#18007 = ORIENTED_EDGE ( 'NONE', *, *, #3556, .T. ) ;
#18008 = ORIENTED_EDGE ( 'NONE', *, *, #555, .T. ) ;
#18009 = VERTEX_POINT ( 'NONE', #18540 ) ;
#18010 = CARTESIAN_POINT ( 'NONE',  ( -85.40000000000000568, -34.91250000000000142, -98.26794919243111792 ) ) ;
#18011 = CARTESIAN_POINT ( 'NONE',  ( -83.25523545990762386, -35.19352049914630953, 96.73097394877602540 ) ) ;
#18012 = AXIS2_PLACEMENT_3D ( 'NONE', #8751, #14703, #10224 ) ;
#18013 = CARTESIAN_POINT ( 'NONE',  ( -85.40000000000000568, -33.05624999877096570, 101.7320508075688679 ) ) ;
#18014 = CARTESIAN_POINT ( 'NONE',  ( 85.40000000000000568, -32.21249999999999858, 98.26794919243111792 ) ) ;
#18015 = EDGE_CURVE ( 'NONE', #6930, #2849, #17361, .T. ) ;
#18016 = PRODUCT_DEFINITION ( 'UNKNOWN', '', #9886, #12171 ) ;
#18017 = CARTESIAN_POINT ( 'NONE',  ( 232.5999999999999375, -32.00000000000000000, 99.99999999999998579 ) ) ;
#18018 = CARTESIAN_POINT ( 'NONE',  ( 231.2217848218749339, -33.81562499938547717, 97.61286128772489690 ) ) ;
#18019 = CARTESIAN_POINT ( 'NONE',  ( 231.2217848218749339, -33.81562499938547717, -52.38713871227520968 ) ) ;
#18020 = AXIS2_PLACEMENT_3D ( 'NONE', #18311, #15472, #8140 ) ;
#18021 = CYLINDRICAL_SURFACE ( 'NONE', #9941, 5.000000000000000000 ) ;
#18022 = CARTESIAN_POINT ( 'NONE',  ( 85.15643035624999868, -30.17812499938548498, -98.40857419181659793 ) ) ;
#18023 = ORIENTED_EDGE ( 'NONE', *, *, #13688, .F. ) ;
#18024 =( BOUNDED_SURFACE ( )  B_SPLINE_SURFACE ( 3, 2, ( 
 ( #4510, #5888, #13491 ),
 ( #12028, #225, #10465 ),
 ( #4613, #6179, #13202 ),
 ( #9092, #31, #17707 ),
 ( #19272, #15055, #19174 ),
 ( #16432, #10372, #4712 ) ),
 .UNSPECIFIED., .F., .F., .F. ) 
 B_SPLINE_SURFACE_WITH_KNOTS ( ( 4, 2, 4 ),
 ( 3, 3 ),
 ( 0.02032853247518126225, 0.02278863295364821212, 0.02524873343211516200 ),
 ( 0.000000000000000000, 1.000000000000000000 ),
 .UNSPECIFIED. ) 
 GEOMETRIC_REPRESENTATION_ITEM ( )  RATIONAL_B_SPLINE_SURFACE ( (
 ( 1.000000000000000000, 0.8047781615896835161, 1.000000000000000000),
 ( 1.000000000000000000, 0.8123767586291043008, 1.000000000000000000),
 ( 1.000000000000000000, 0.8190662415562011134, 1.000000000000000000),
 ( 1.000000000000000000, 0.8192361015671398849, 1.000000000000000000),
 ( 1.000000000000000000, 0.8126135807102121689, 1.000000000000000000),
 ( 1.000000000000000000, 0.8047712338318585568, 1.000000000000000000) ) ) 
 REPRESENTATION_ITEM ( '' )  SURFACE ( )  );
#18025 = CARTESIAN_POINT ( 'NONE',  ( 232.5999999999999375, -33.26249999999999574, -53.46410161513786363 ) ) ;
#18026 = CARTESIAN_POINT ( 'NONE',  ( -82.40000000000000568, -33.93750000000000711, 102.9999999999999858 ) ) ;
#18027 = CARTESIAN_POINT ( 'NONE',  ( 79.64356964375001269, -34.45312499938548711, -101.5914258081833879 ) ) ;
#18028 = AXIS2_PLACEMENT_3D ( 'NONE', #7054, #14281, #821 ) ;
#18029 = CARTESIAN_POINT ( 'NONE',  ( 0.1217565302851095904, 2.351289329882149559, 2.927447417349536618 ) ) ;
#18030 = CARTESIAN_POINT ( 'NONE',  ( 81.59615242270662350, -33.73259618943233562, -96.99999999999998579 ) ) ;
#18031 = CARTESIAN_POINT ( 'NONE',  ( -79.39999999999999147, -34.76250000000000284, 101.7320508075688537 ) ) ;
#18032 = CARTESIAN_POINT ( 'NONE',  ( -79.39999999999999147, -31.61250000000000071, 101.7320508075688537 ) ) ;
#18033 = VERTEX_POINT ( 'NONE', #2501 ) ;
#18034 = CARTESIAN_POINT ( 'NONE',  ( -85.32499745258149915, -34.99999999999999289, 99.84129707247753061 ) ) ;
#18035 = VECTOR ( 'NONE', #329, 1000.000000000000000 ) ;
#18036 = CARTESIAN_POINT ( 'NONE',  ( -82.40000000000000568, -34.38749999999999574, 102.9999999999999858 ) ) ;
#18037 = CARTESIAN_POINT ( 'NONE',  ( 81.02178482187500208, -30.89062499938548711, 97.61286128772489690 ) ) ;
#18038 = CARTESIAN_POINT ( 'NONE',  ( -80.90000000000000568, -32.99606250001229313, 102.5980762113533018 ) ) ;
#18039 = VECTOR ( 'NONE', #7724, 1000.000000000000000 ) ;
#18040 = AXIS2_PLACEMENT_3D ( 'NONE', #16665, #1808, #15390 ) ;
#18041 = LINE ( 'NONE', #4652, #3603 ) ;
#18042 = CARTESIAN_POINT ( 'NONE',  ( 235.3140393761304665, -32.00000000000000000, -48.72172371342785624 ) ) ;
#18043 = CARTESIAN_POINT ( 'NONE',  ( 5.599999999999999645, 0.000000000000000000, 0.000000000000000000 ) ) ;
#18044 = CARTESIAN_POINT ( 'NONE',  ( 85.15643035625001289, -30.59062499938548285, 99.99999999999998579 ) ) ;
#18045 = CARTESIAN_POINT ( 'NONE',  ( 85.15643035624999868, -30.29062499938548925, -98.40857419181659793 ) ) ;
#18046 = AXIS2_PLACEMENT_3D ( 'NONE', #14116, #18627, #12946 ) ;
#18047 = DIRECTION ( 'NONE',  ( -0.000000000000000000, -0.000000000000000000, -1.000000000000000000 ) ) ;
#18048 = CARTESIAN_POINT ( 'NONE',  ( -84.53225329756183726, -32.00000000000000000, -101.7559005160110956 ) ) ;
#18049 = CARTESIAN_POINT ( 'NONE',  ( -83.77821517812500929, -31.07812499938548711, -97.61286128772489690 ) ) ;
#18050 = ORIENTED_EDGE ( 'NONE', *, *, #2229, .T. ) ;
#18051 = CARTESIAN_POINT ( 'NONE',  ( 81.02178482187500208, -31.45312499938549067, 97.61286128772489690 ) ) ;
#18052 = CARTESIAN_POINT ( 'NONE',  ( -1.317756351988340180, 3.857995168970202116, -0.04852650426601388955 ) ) ;
#18053 = VECTOR ( 'NONE', #5410, 1000.000000000000000 ) ;
#18054 = AXIS2_PLACEMENT_3D ( 'NONE', #13053, #19019, #5640 ) ;
#18055 = CARTESIAN_POINT ( 'NONE',  ( -81.02178482187500208, -30.85312499938548569, 97.61286128772489690 ) ) ;
#18056 =( BOUNDED_CURVE ( )  B_SPLINE_CURVE ( 2, ( #6503, #18226, #12638, #5131, #18514, #11076, #5229 ),
 .UNSPECIFIED., .F., .T. ) 
 B_SPLINE_CURVE_WITH_KNOTS ( ( 3, 2, 2, 3 ),
 ( 0.3702305174531529408, 0.3750000000000000000, 0.3888888888888888951, 0.3958333333333334259 ),
 .UNSPECIFIED. ) 
 CURVE ( )  GEOMETRIC_REPRESENTATION_ITEM ( )  RATIONAL_B_SPLINE_CURVE ( ( 0.9395835397632826824, 0.9539927561172878434, 1.000000000000000000, 0.8660254037844387076, 1.000000000000000000, 0.9330127018922185211, 0.9330127018922192983 ) ) 
 REPRESENTATION_ITEM ( '' )  );
#18057 = ORIENTED_EDGE ( 'NONE', *, *, #3143, .T. ) ;
#18058 = CARTESIAN_POINT ( 'NONE',  ( -85.40000000000000568, -32.21249999999999858, -98.26794919243111792 ) ) ;
#18059 = CARTESIAN_POINT ( 'NONE',  ( 0.000000000000000000, 0.000000000000000000, 0.000000000000000000 ) ) ;
#18060 = CARTESIAN_POINT ( 'NONE',  ( -83.77821517812500929, -32.57812499938548711, -102.3871387122750889 ) ) ;
#18061 = DIRECTION ( 'NONE',  ( 0.000000000000000000, 0.000000000000000000, 1.000000000000000000 ) ) ;
#18062 = CARTESIAN_POINT ( 'NONE',  ( 235.3564303562499447, -31.86562499938547788, 101.5914258081833879 ) ) ;
#18063 = CARTESIAN_POINT ( 'NONE',  ( -79.39999999999999147, -32.87268749875867968, 99.99999999999998579 ) ) ;
#18064 = CARTESIAN_POINT ( 'NONE',  ( -81.02178482187500208, -34.15312499938548285, 102.3871387122750889 ) ) ;
#18065 = CYLINDRICAL_SURFACE ( 'NONE', #18822, 3.000000000000002665 ) ;
#18066 = CARTESIAN_POINT ( 'NONE',  ( 79.64356964374998427, -33.55312499938548854, 98.40857419181659793 ) ) ;
#18067 = CARTESIAN_POINT ( 'NONE',  ( 105.1999999999999744, -31.99999999999999289, 150.0000000000000000 ) ) ;
#18068 = CARTESIAN_POINT ( 'NONE',  ( 233.4038475772932770, -33.41115380933862156, 103.0000000000000000 ) ) ;
#18069 = CARTESIAN_POINT ( 'NONE',  ( 83.90000000000000568, -33.61874999877097281, -97.40192378864668399 ) ) ;
#18070 = CARTESIAN_POINT ( 'NONE',  ( 231.0999999999999375, -33.22499999999999432, 97.40192378864668399 ) ) ;
#18071 = ADVANCED_FACE ( 'NONE', ( #15706 ), #5359, .T. ) ;
#18072 = ADVANCED_FACE ( 'NONE', ( #3775 ), #15459, .F. ) ;
#18073 = EDGE_LOOP ( 'NONE', ( #9487, #13952, #14075, #507 ) ) ;
#18074 = CARTESIAN_POINT ( 'NONE',  ( 229.8435696437499587, -32.99062499938548143, -51.59142580818350154 ) ) ;
#18075 = DIRECTION ( 'NONE',  ( -1.000000000000000000, -1.336382355046098552E-47, 4.814824860968092260E-31 ) ) ;
#18076 = CARTESIAN_POINT ( 'NONE',  ( 231.0999999999999375, -34.81874999877096144, 102.5980762113533018 ) ) ;
#18077 = CARTESIAN_POINT ( 'NONE',  ( 233.9782151781249411, -31.30312499938547788, -52.38713871227520968 ) ) ;
#18078 = CARTESIAN_POINT ( 'NONE',  ( -82.39999999999999147, -33.62812499938548427, 103.1828516163667899 ) ) ;
#18079 = ORIENTED_EDGE ( 'NONE', *, *, #5066, .F. ) ;
#18080 = ORIENTED_EDGE ( 'NONE', *, *, #13335, .F. ) ;
#18081 = CARTESIAN_POINT ( 'NONE',  ( 4.158413352280814657, 2.044871626972823986, -3.541821552872970180 ) ) ;
#18082 = CARTESIAN_POINT ( 'NONE',  ( -99.99999999999998579, -32.00000000000000000, 150.0000000000000000 ) ) ;
#18083 = CARTESIAN_POINT ( 'NONE',  ( 5.100000000000002309, 0.000000000000000000, 0.000000000000000000 ) ) ;
#18084 = ORIENTED_EDGE ( 'NONE', *, *, #162, .F. ) ;
#18085 = FACE_OUTER_BOUND ( 'NONE', #9293, .T. ) ;
#18086 = CARTESIAN_POINT ( 'NONE',  ( 113.0000000000000142, 10.19999999999997264, -145.0000000000000000 ) ) ;
#18087 = EDGE_CURVE ( 'NONE', #10401, #4006, #11853, .T. ) ;
#18088 = CARTESIAN_POINT ( 'NONE',  ( -82.39999999999999147, -34.19062499938548427, 103.1828516163667899 ) ) ;
#18089 = CARTESIAN_POINT ( 'NONE',  ( -79.39999999999999147, -30.58124999877096784, 98.26794919243110371 ) ) ;
#18090 = CARTESIAN_POINT ( 'NONE',  ( -83.90000000000000568, -31.36874999877096926, 97.40192378864668399 ) ) ;
#18091 = CARTESIAN_POINT ( 'NONE',  ( 232.5999999999999375, -33.71249999999999147, 96.99999999999998579 ) ) ;
#18092 =( BOUNDED_CURVE ( )  B_SPLINE_CURVE ( 2, ( #13822, #4954, #10896, #3470, #6515, #14208, #944, #6900, #6991 ),
 .UNSPECIFIED., .F., .F. ) 
 B_SPLINE_CURVE_WITH_KNOTS ( ( 3, 2, 2, 2, 3 ),
 ( 0.3958333333333333148, 0.4027777777777777901, 0.4166666666666666852, 0.4305555555555555802, 0.4374999999999999445 ),
 .UNSPECIFIED. ) 
 CURVE ( )  GEOMETRIC_REPRESENTATION_ITEM ( )  RATIONAL_B_SPLINE_CURVE ( ( 0.9330127018922194093, 0.9330127018922190762, 1.000000000000000000, 0.8660254037844387076, 1.000000000000000000, 0.8660254037844387076, 1.000000000000000000, 0.9330127018922198534, 0.9330127018922192983 ) ) 
 REPRESENTATION_ITEM ( '' )  );
#18093 = CARTESIAN_POINT ( 'NONE',  ( -81.59615242270662350, -33.91740381056766296, 103.0000000000000000 ) ) ;
#18094 = CARTESIAN_POINT ( 'NONE',  ( 232.5999999999999375, -33.26249999999999574, 97.00000000000000000 ) ) ;
#18095 = DIRECTION ( 'NONE',  ( -0.000000000000000000, -1.000000000000000000, -0.000000000000000000 ) ) ;
#18096 = CARTESIAN_POINT ( 'NONE',  ( 4.000000000000000000, -1.942223658245635809, -0.3516579909967643691 ) ) ;
#18097 = EDGE_CURVE ( 'NONE', #10162, #11406, #14931, .T. ) ;
#18098 = CARTESIAN_POINT ( 'NONE',  ( 233.9782151781249411, -31.64062499938547646, 97.61286128772489690 ) ) ;
#18099 = VERTEX_POINT ( 'NONE', #10107 ) ;
#18100 = CARTESIAN_POINT ( 'NONE',  ( -82.39999999999999147, -33.62812499938549138, -96.81714838363319586 ) ) ;
#18101 = CARTESIAN_POINT ( 'NONE',  ( 234.0999999999999375, -32.54999999999999716, -47.40192378864679768 ) ) ;
#18102 = FACE_OUTER_BOUND ( 'NONE', #15322, .T. ) ;
#18103 = CARTESIAN_POINT ( 'NONE',  ( 79.90595866893272614, -34.99999999999998579, -101.1871036926522578 ) ) ;
#18104 = FACE_BOUND ( 'NONE', #6088, .T. ) ;
#18105 = CARTESIAN_POINT ( 'NONE',  ( 231.2217848218749339, -34.71562499938547575, -52.38713871227520968 ) ) ;
#18106 = ORIENTED_EDGE ( 'NONE', *, *, #6312, .T. ) ;
#18107 = EDGE_LOOP ( 'NONE', ( #3597, #17210, #10069, #7826 ) ) ;
#18108 = CARTESIAN_POINT ( 'NONE',  ( -99.99999999999998579, -32.00000000000000000, 150.0000000000000000 ) ) ;
#18109 = CARTESIAN_POINT ( 'NONE',  ( -82.39999999999999147, -30.56250000000000355, 96.53589838486223584 ) ) ;
#18110 = CARTESIAN_POINT ( 'NONE',  ( -79.39999999999999147, -32.83124999877097139, 98.26794919243110371 ) ) ;
#18111 = CARTESIAN_POINT ( 'NONE',  ( 83.90000000000000568, -32.62500000000000000, 97.40192378864668399 ) ) ;
#18112 = CARTESIAN_POINT ( 'NONE',  ( 85.40000000000000568, -33.50624999877096855, 98.26794919243111792 ) ) ;
#18113 = CARTESIAN_POINT ( 'NONE',  ( 231.2217848218749339, -32.76562499938548001, 102.3871387122750889 ) ) ;
#18114 = CARTESIAN_POINT ( 'NONE',  ( 81.02178482187500208, -33.70312499938548711, -102.3871387122750889 ) ) ;
#18115 = DIRECTION ( 'NONE',  ( 0.000000000000000000, -1.000000000000000000, 0.000000000000000000 ) ) ;
#18116 = CARTESIAN_POINT ( 'NONE',  ( 83.77821517812500929, -33.36562499938548854, -97.61286128772489690 ) ) ;
#18117 = ORIENTED_EDGE ( 'NONE', *, *, #17971, .T. ) ;
#18118 = CARTESIAN_POINT ( 'NONE',  ( 231.0999999999999375, -32.77499999999999147, -52.59807621135342970 ) ) ;
#18119 = CARTESIAN_POINT ( 'NONE',  ( -79.64356964374998427, -34.90312499938548285, 101.5914258081833879 ) ) ;
#18120 = CARTESIAN_POINT ( 'NONE',  ( 79.64356964375001269, -34.00312499938549138, -101.5914258081833879 ) ) ;
#18121 = CARTESIAN_POINT ( 'NONE',  ( -82.39999999999999147, -32.98124999877096286, 102.9999999999999858 ) ) ;
#18122 = CARTESIAN_POINT ( 'NONE',  ( -79.64356964375001269, -31.86562499938548143, 101.5914258081833879 ) ) ;
#18123 = ADVANCED_FACE ( 'NONE', ( #10199 ), #16063, .T. ) ;
#18124 = CARTESIAN_POINT ( 'NONE',  ( 232.5999999999999375, -32.16562499938547859, -53.18285161636690361 ) ) ;
#18125 = CARTESIAN_POINT ( 'NONE',  ( -79.39999999999999147, -30.63750000000000284, 98.26794919243110371 ) ) ;
#18126 = ORIENTED_EDGE ( 'NONE', *, *, #2537, .F. ) ;
#18127 = CARTESIAN_POINT ( 'NONE',  ( -79.77381699087979428, -34.99985067802517591, 101.4917037897926093 ) ) ;
#18128 = PLANE ( 'NONE',  #1111 ) ;
#18129 = CARTESIAN_POINT ( 'NONE',  ( -85.40000000000000568, -30.86250000000000071, 101.7320508075688679 ) ) ;
#18130 = CARTESIAN_POINT ( 'NONE',  ( 0.1388410611046122789, -3.710337782248038785, -0.5735064479039801988 ) ) ;
#18131 = CARTESIAN_POINT ( 'NONE',  ( -81.02178482187500208, -32.20312499938548711, 97.61286128772489690 ) ) ;
#18132 = CARTESIAN_POINT ( 'NONE',  ( 232.5999999999999659, -32.13749999999999574, 102.9999999999999858 ) ) ;
#18133 = CARTESIAN_POINT ( 'NONE',  ( 82.39999999999999147, -34.41562499938547859, 103.1828516163667899 ) ) ;
#18134 = EDGE_CURVE ( 'NONE', #19014, #11146, #8482, .T. ) ;
#18135 = CARTESIAN_POINT ( 'NONE',  ( 81.02178482187500208, -32.65312499938548996, -97.61286128772489690 ) ) ;
#18136 = CARTESIAN_POINT ( 'NONE',  ( 235.3564303562499447, -31.71562499938547575, -50.00000000000011369 ) ) ;
#18137 = CARTESIAN_POINT ( 'NONE',  ( -85.15643035625001289, -32.50312499938548427, 99.99999999999998579 ) ) ;
#18138 = CARTESIAN_POINT ( 'NONE',  ( -85.15643035624999868, -34.79062499938548569, -101.5914258081833879 ) ) ;
#18139 =( BOUNDED_SURFACE ( )  B_SPLINE_SURFACE ( 3, 2, ( 
 ( #15579, #8047, #14004 ),
 ( #642, #6592, #8336 ),
 ( #18510, #5128, #17041 ),
 ( #2190, #18608, #11172 ),
 ( #17139, #3744, #2280 ),
 ( #8244, #14195, #1467 ) ),
 .UNSPECIFIED., .F., .F., .F. ) 
 B_SPLINE_SURFACE_WITH_KNOTS ( ( 4, 2, 4 ),
 ( 3, 3 ),
 ( 0.01651732063679904258, 0.01857756227444016389, 0.02063780391208128520 ),
 ( 0.000000000000000000, 1.000000000000000000 ),
 .UNSPECIFIED. ) 
 GEOMETRIC_REPRESENTATION_ITEM ( )  RATIONAL_B_SPLINE_SURFACE ( (
 ( 1.000000000000000000, 0.8047781231227483234, 1.000000000000000000),
 ( 1.000000000000000000, 0.8123782108664980850, 1.000000000000000000),
 ( 1.000000000000000000, 0.8190665102133478648, 1.000000000000000000),
 ( 1.000000000000000000, 0.8192358432844011329, 1.000000000000000000),
 ( 1.000000000000000000, 0.8126132624435309371, 1.000000000000000000),
 ( 1.000000000000000000, 0.8047712436238877443, 1.000000000000000000) ) ) 
 REPRESENTATION_ITEM ( '' )  SURFACE ( )  );
#18140 = ORIENTED_EDGE ( 'NONE', *, *, #7977, .T. ) ;
#18141 = CARTESIAN_POINT ( 'NONE',  ( 81.02178482187500208, -30.55312499938548854, 97.61286128772489690 ) ) ;
#18142 = CARTESIAN_POINT ( 'NONE',  ( 85.40000000000000568, -34.40624999877096712, 98.26794919243111792 ) ) ;
#18143 = CARTESIAN_POINT ( 'NONE',  ( 4.170895651974600327, -2.054890354522638685, -3.559174498016469457 ) ) ;
#18144 = CARTESIAN_POINT ( 'NONE',  ( -79.64356964375001269, -30.51562499938548711, 101.5914258081833879 ) ) ;
#18145 = CARTESIAN_POINT ( 'NONE',  ( 232.5999999999999659, -32.53124999877096712, 103.0000000000000000 ) ) ;
#18146 = ORIENTED_EDGE ( 'NONE', *, *, #17135, .T. ) ;
#18147 = CARTESIAN_POINT ( 'NONE',  ( -79.39999999999999147, -30.22500000000000142, -99.99999999999998579 ) ) ;
#18148 = LINE ( 'NONE', #16771, #11612 ) ;
#18149 = FACE_OUTER_BOUND ( 'NONE', #8951, .T. ) ;
#18150 = CARTESIAN_POINT ( 'NONE',  ( -85.15643035625001289, -34.30312499938548854, -99.99999999999998579 ) ) ;
#18151 = CARTESIAN_POINT ( 'NONE',  ( 234.0999999999999375, -32.79374999877096286, -52.59807621135342970 ) ) ;
#18152 = CARTESIAN_POINT ( 'NONE',  ( 229.8435696437499303, -34.75312499938547717, 99.99999999999998579 ) ) ;
#18153 = CARTESIAN_POINT ( 'NONE',  ( -82.39999999999999147, -31.86018749875867684, 96.53589838486223584 ) ) ;
#18154 = ORIENTED_EDGE ( 'NONE', *, *, #13289, .T. ) ;
#18155 = CARTESIAN_POINT ( 'NONE',  ( 110.0000000000000000, 10.19999999999997620, -145.0000000000000000 ) ) ;
#18156 = CARTESIAN_POINT ( 'NONE',  ( -82.39999999999999147, -33.65624999877097423, 97.00000000000000000 ) ) ;
#18157 = CARTESIAN_POINT ( 'NONE',  ( 85.15643035625001289, -32.80312499938548854, 98.40857419181659793 ) ) ;
#18158 = CARTESIAN_POINT ( 'NONE',  ( 83.90000000000000568, -34.51874999877097139, -97.40192378864668399 ) ) ;
#18159 = CARTESIAN_POINT ( 'NONE',  ( -82.40000000000001990, -34.55624999877097281, 97.00000000000000000 ) ) ;
#18160 = CARTESIAN_POINT ( 'NONE',  ( 80.90000000000000568, -33.84374999877096712, -102.5980762113533018 ) ) ;
#18161 = CARTESIAN_POINT ( 'NONE',  ( 81.59615242270662350, -34.63259618943234130, 103.0000000000000000 ) ) ;
#18162 = AXIS2_PLACEMENT_3D ( 'NONE', #6564, #15742, #11242 ) ;
#18163 = ORIENTED_EDGE ( 'NONE', *, *, #11869, .F. ) ;
#18164 = CARTESIAN_POINT ( 'NONE',  ( 233.9782151781249411, -33.70312499938548001, -47.61286128772501769 ) ) ;
#18165 = DIRECTION ( 'NONE',  ( 0.000000000000000000, 0.000000000000000000, 1.000000000000000000 ) ) ;
#18166 = CARTESIAN_POINT ( 'NONE',  ( 235.3564303562499447, -30.96562499938547930, 101.5914258081833879 ) ) ;
#18167 = CARTESIAN_POINT ( 'NONE',  ( 235.3564303562499447, -30.44062499938548072, -51.59142580818350865 ) ) ;
#18168 = CARTESIAN_POINT ( 'NONE',  ( -82.40000000000000568, -33.03750000000000142, -96.99999999999998579 ) ) ;
#18169 = VERTEX_POINT ( 'NONE', #7937 ) ;
#18170 = ORIENTED_EDGE ( 'NONE', *, *, #1725, .F. ) ;
#18171 = CARTESIAN_POINT ( 'NONE',  ( 231.0999999999999375, -32.56874999877096144, -47.40192378864679768 ) ) ;
#18172 = CARTESIAN_POINT ( 'NONE',  ( 231.7961524227065979, -34.85759618943232852, 103.0000000000000000 ) ) ;
#18173 = CARTESIAN_POINT ( 'NONE',  ( -81.59615242270662350, -34.63259618943234130, 96.99999999999997158 ) ) ;
#18174 = ORIENTED_EDGE ( 'NONE', *, *, #11911, .F. ) ;
#18175 = CARTESIAN_POINT ( 'NONE',  ( -6.473970235329672780E-16, -4.862606272033106691, -3.745885042887442395 ) ) ;
#18176 = CARTESIAN_POINT ( 'NONE',  ( -99.99999999999998579, -5.200000000000000178, 150.0000000000000000 ) ) ;
#18177 = AXIS2_PLACEMENT_3D ( 'NONE', #8148, #6399, #14099 ) ;
#18178 = AXIS2_PLACEMENT_3D ( 'NONE', #5531, #943, #5442 ) ;
#18179 = LINE ( 'NONE', #11028, #4141 ) ;
#18180 = CARTESIAN_POINT ( 'NONE',  ( -82.39999999999999147, -30.50624999877097210, 96.53589838486223584 ) ) ;
#18181 = CARTESIAN_POINT ( 'NONE',  ( -82.39999999999999147, -31.63124999877097210, 103.4641016151377499 ) ) ;
#18182 = DIRECTION ( 'NONE',  ( -0.8660254037844373753, 0.5000000000000021094, 0.000000000000000000 ) ) ;
#18183 = DIRECTION ( 'NONE',  ( 0.000000000000000000, 0.000000000000000000, 1.000000000000000000 ) ) ;
#18184 = SURFACE_STYLE_USAGE ( .BOTH. , #12313 ) ;
#18185 = LINE ( 'NONE', #1673, #2130 ) ;
#18186 = CARTESIAN_POINT ( 'NONE',  ( -79.39999999999999147, -34.63124999877096855, -101.7320508075688963 ) ) ;
#18187 = CARTESIAN_POINT ( 'NONE',  ( 232.5999999999999375, -32.50312499938547717, 96.81714838363319586 ) ) ;
#18188 = ORIENTED_EDGE ( 'NONE', *, *, #15209, .F. ) ;
#18189 = SURFACE_SIDE_STYLE ('',( #15342 ) ) ;
#18190 = CARTESIAN_POINT ( 'NONE',  ( -81.02178482187500208, -32.54062499938548569, -102.3871387122750889 ) ) ;
#18191 = DIRECTION ( 'NONE',  ( -4.625929269271485174E-17, -1.000000000000000000, 0.000000000000000000 ) ) ;
#18192 = EDGE_CURVE ( 'NONE', #13276, #1546, #15873, .T. ) ;
#18193 = VECTOR ( 'NONE', #9443, 1000.000000000000000 ) ;
#18194 = ORIENTED_EDGE ( 'NONE', *, *, #2354, .F. ) ;
#18195 = DIRECTION ( 'NONE',  ( 0.000000000000000000, -1.000000000000000000, 0.000000000000000000 ) ) ;
#18196 = CYLINDRICAL_SURFACE ( 'NONE', #3054, 6.000000000000005329 ) ;
#18197 = CARTESIAN_POINT ( 'NONE',  ( 231.7960411235079050, -35.00000000000002132, -47.36341917746382535 ) ) ;
#18198 = DIRECTION ( 'NONE',  ( 0.000000000000000000, 0.000000000000000000, -1.000000000000000000 ) ) ;
#18199 = ORIENTED_EDGE ( 'NONE', *, *, #15488, .F. ) ;
#18200 = ORIENTED_EDGE ( 'NONE', *, *, #16679, .F. ) ;
#18201 = CARTESIAN_POINT ( 'NONE',  ( -82.39076102795759482, -32.00000000000002132, 102.8695224571928719 ) ) ;
#18202 = CARTESIAN_POINT ( 'NONE',  ( 85.15643035624999868, -35.11426541925033007, -98.99674735228809652 ) ) ;
#18203 = EDGE_CURVE ( 'NONE', #8568, #1717, #7550, .T. ) ;
#18204 = CARTESIAN_POINT ( 'NONE',  ( -79.39999999999999147, -31.51874999877096784, 99.99999999999998579 ) ) ;
#18205 = CARTESIAN_POINT ( 'NONE',  ( 85.40000000000000568, -32.73750000000000426, 101.7320508075688679 ) ) ;
#18206 = DIRECTION ( 'NONE',  ( 1.000000000000000000, -0.000000000000000000, -2.407412430484046130E-31 ) ) ;
#18208 = CARTESIAN_POINT ( 'NONE',  ( 229.8435696437499871, -32.80312499938548143, 101.5914258081833879 ) ) ;
#18207 = AXIS2_PLACEMENT_3D ( 'NONE', #8393, #1167, #17485 ) ;
#18209 = CARTESIAN_POINT ( 'NONE',  ( 85.15643035625001289, -33.81562499938548427, -101.5914258081833879 ) ) ;
#18210 = CARTESIAN_POINT ( 'NONE',  ( 96.99999999999994316, -29.80000000000000426, 150.0000000000000000 ) ) ;
#18211 = CARTESIAN_POINT ( 'NONE',  ( 85.15643035624999868, -33.77812499938548285, -98.40857419181659793 ) ) ;
#18212 = ORIENTED_EDGE ( 'NONE', *, *, #16643, .T. ) ;
#18213 = CARTESIAN_POINT ( 'NONE',  ( 232.5999999999999375, -31.68749999999999289, -46.53589838486234953 ) ) ;
#18214 = CARTESIAN_POINT ( 'NONE',  ( 83.77821517812500929, -32.46562499938548285, -97.61286128772489690 ) ) ;
#18215 = PLANE ( 'NONE',  #10835 ) ;
#18216 = EDGE_CURVE ( 'NONE', #18536, #2292, #16484, .T. ) ;
#18217 = FACE_OUTER_BOUND ( 'NONE', #3504, .T. ) ;
#18218 = CARTESIAN_POINT ( 'NONE',  ( -82.39999999999999147, -30.81562499938548427, 96.81714838363319586 ) ) ;
#18219 = CARTESIAN_POINT ( 'NONE',  ( 231.2217848218749339, -34.22812499938548569, -47.61286128772501769 ) ) ;
#18220 = EDGE_CURVE ( 'NONE', #867, #4201, #6013, .T. ) ;
#18221 = CARTESIAN_POINT ( 'NONE',  ( -85.40000000000000568, -30.48749999999999716, 98.26794919243111792 ) ) ;
#18222 = ORIENTED_EDGE ( 'NONE', *, *, #13804, .T. ) ;
#18223 = CARTESIAN_POINT ( 'NONE',  ( 232.3466685930879123, -34.99995246259152282, 97.01071553687879145 ) ) ;
#18224 = CARTESIAN_POINT ( 'NONE',  ( -79.39999999999999147, -31.06874999877096855, 99.99999999999998579 ) ) ;
#18225 = DIRECTION ( 'NONE',  ( -0.000000000000000000, -1.000000000000000000, -0.000000000000000000 ) ) ;
#18226 = CARTESIAN_POINT ( 'NONE',  ( 79.40000000000000568, -32.01330983656912821, -99.46005447970492241 ) ) ;
#18227 = ADVANCED_FACE ( 'NONE', ( #10769 ), #4633, .T. ) ;
#18228 = CARTESIAN_POINT ( 'NONE',  ( -81.02178482187500208, -31.45312499938549067, 102.3871387122750889 ) ) ;
#18229 = CARTESIAN_POINT ( 'NONE',  ( 79.93183330737453218, -31.99999999999997158, 98.31447495408103521 ) ) ;
#18230 = CARTESIAN_POINT ( 'NONE',  ( 81.02178482187500208, -34.45312499938548711, 102.3871387122750889 ) ) ;
#18231 = CARTESIAN_POINT ( 'NONE',  ( 82.39999999999999147, -32.84062499938548996, -103.1828516163667899 ) ) ;
#18232 = CARTESIAN_POINT ( 'NONE',  ( 235.3564303562499447, -30.85312499938547859, -48.40857419181671162 ) ) ;
#18233 = CARTESIAN_POINT ( 'NONE',  ( -85.15643035625001289, -33.81562499938548427, 101.5914258081833879 ) ) ;
#18234 = CARTESIAN_POINT ( 'NONE',  ( -79.64356964374999848, -33.62812499938548427, -99.99999999999998579 ) ) ;
#18235 = VERTEX_POINT ( 'NONE', #3058 ) ;
#18236 = CARTESIAN_POINT ( 'NONE',  ( 79.64356964375001269, -30.51562499938548711, 98.40857419181659793 ) ) ;
#18237 = CARTESIAN_POINT ( 'NONE',  ( 235.5999999999999375, -34.27499999999999147, 99.99999999999998579 ) ) ;
#18238 = FILL_AREA_STYLE_COLOUR ( '', #8340 ) ;
#18239 = CARTESIAN_POINT ( 'NONE',  ( -85.15643035624999868, -33.81562499938549138, 101.5914258081833879 ) ) ;
#18240 = CARTESIAN_POINT ( 'NONE',  ( 111.0000000000000000, 15.19999999999997620, -136.6833752096445380 ) ) ;
#18241 = ORIENTED_EDGE ( 'NONE', *, *, #4863, .F. ) ;
#18242 = ADVANCED_FACE ( 'NONE', ( #15362 ), #18021, .T. ) ;
#18243 = CARTESIAN_POINT ( 'NONE',  ( -79.39999999999999147, -31.98750000000000071, -101.7320508075688821 ) ) ;
#18244 = CARTESIAN_POINT ( 'NONE',  ( 84.12112955302457351, -35.00000000000000000, 102.4658001909610476 ) ) ;
#18245 = CARTESIAN_POINT ( 'NONE',  ( -0.6920835326022555245, -4.454600218803899558, -3.597382984111586079 ) ) ;
#18246 = CARTESIAN_POINT ( 'NONE',  ( -83.77821517812500929, -34.82812499938548711, -102.3871387122750889 ) ) ;
#18247 = CARTESIAN_POINT ( 'NONE',  ( 235.5999999999999943, -32.90624999877096002, -48.26794919243124582 ) ) ;
#18248 = CARTESIAN_POINT ( 'NONE',  ( 233.9782151781249411, -35.05312499938548143, 102.3871387122750889 ) ) ;
#18249 = CARTESIAN_POINT ( 'NONE',  ( -83.90000000000000568, -34.82268749875867542, 102.5980762113533018 ) ) ;
#18250 = ORIENTED_EDGE ( 'NONE', *, *, #12736, .T. ) ;
#18251 = ADVANCED_FACE ( 'NONE', ( #3344 ), #14980, .F. ) ;
#18252 = DIRECTION ( 'NONE',  ( 0.000000000000000000, -1.000000000000000000, 0.000000000000000000 ) ) ;
#18253 = CARTESIAN_POINT ( 'NONE',  ( 83.90000000000000568, -32.32500000000000284, 102.5980762113533018 ) ) ;
#18254 = CARTESIAN_POINT ( 'NONE',  ( 79.64356964374999848, -33.51562499938548711, 99.99999999999998579 ) ) ;
#18255 = CARTESIAN_POINT ( 'NONE',  ( 81.59615242270662350, -34.36740381056766580, 96.99999999999998579 ) ) ;
#18256 =( BOUNDED_CURVE ( )  B_SPLINE_CURVE ( 2, ( #8693, #11241, #17205, #12804, #2731, #4014, #16124, #17399, #3809, #899, #18868, #15741, #9976, #2347, #16026, #2449, #10067, #14261, #12901, #14448, #13088, #2532, #6859, #8591, #6948, #14643, #14356, #8493, #6761, #18771, #5393, #1179, #12704, #7038, #7137, #3909, #1081, #11338, #15837, #4106, #17303, #8404, #18965, #5587, #11534, #2627, #18677, #19058, #5680, #9876, #11623, #17588, #4200, #10160, #5490, #5295, #11437, #13180, #7225, #8785, #6156, #5961, #17978, #1375, #10637, #6060, #3112, #14740, #12006, #4589, #13274, #7321, #9071, #17685, #1277, #12105, #13562, #10547, #16509, #109, #3018, #10445, #17787, #15035, #1658, #7610, #203, #9168, #19249, #16316, #4394, #19152, #7417, #18078, #10351, #14837, #4686, #5765, #10262, #1463, #16603, #8976, #2926, #3209, #11717, #12, #4298, #16225, #13378, #2831, #7513, #5866, #11818, #16409, #8878, #11909, #1567, #14942, #17882, #4490, #13470, #9263, #9360, #4984, #7803, #13950, #16983, #14049, #3406, #12299, #3304, #304, #1845, #11114, #6253 ),
 .UNSPECIFIED., .F., .F. ) 
 B_SPLINE_CURVE_WITH_KNOTS ( ( 3, 2, 2, 2, 2, 2, 2, 2, 2, 2, 2, 2, 2, 2, 2, 2, 2, 2, 2, 2, 2, 2, 2, 2, 2, 2, 2, 2, 2, 2, 2, 2, 2, 2, 2, 2, 2, 2, 2, 2, 2, 2, 2, 2, 2, 2, 2, 2, 2, 2, 2, 2, 2, 2, 2, 2, 2, 2, 2, 2, 2, 2, 2, 2, 2, 2, 2, 3 ),
 ( 0.000000000000000000, 0.01500076742380701197, 0.03000153484761402395, 0.04500230227142103939, 0.06000306969522804790, 0.07500383711903506334, 0.09000460454284207878, 0.1050053719666490942, 0.1200061393904560958, 0.1350069068142631112, 0.1500076742380701267, 0.1650084416618771699, 0.1800092090856841576, 0.1950099765094911730, 0.2100107439332981885, 0.2250115113571052039, 0.2400122787809121916, 0.2550130462047192070, 0.2700138136285262225, 0.2850145810523332379, 0.3000153484761402534, 0.3150161158999473243, 0.3300168833237543398, 0.3450176507475612997, 0.3600184181713683151, 0.3750191855951753306, 0.3900199530189823460, 0.4050207204427893615, 0.4200214878665963769, 0.4350222552904033924, 0.4500230227142104078, 0.4650237901380174232, 0.4800245575618243832, 0.4950253249856313986, 0.5100260924094384141, 0.5250268598332454850, 0.5400276272570524450, 0.5550283946808594049, 0.5700291621046664758, 0.5850299295284734358, 0.6000306969522805067, 0.6150314643760874667, 0.6300322317998946486, 0.6450329992237016086, 0.6600337666475086795, 0.6750345340713156395, 0.6900353014951225994, 0.7050360689189296703, 0.7200368363427366303, 0.7350376037665437012, 0.7500383711903506612, 0.7650391386141577321, 0.7800399060379646921, 0.7950406734617717630, 0.8100414408855787229, 0.8250422083093856829, 0.8400429757331927538, 0.8550437431569997138, 0.8700445105808067847, 0.8850452780046137446, 0.9000460454284208156, 0.9150468128522277755, 0.9300475802760348465, 0.9450483476998418064, 0.9600491151236487664, 0.9750498825474558373, 0.9900506499712627972, 1.000000000000000000 ),
 .UNSPECIFIED. ) 
 CURVE ( )  GEOMETRIC_REPRESENTATION_ITEM ( )  RATIONAL_B_SPLINE_CURVE ( ( 1.000000000000000000, 0.8660254037844387076, 1.000000000000000000, 0.8660254037844387076, 1.000000000000000000, 0.8660254037844387076, 1.000000000000000000, 0.8660254037844387076, 1.000000000000000000, 0.8660254037844387076, 1.000000000000000000, 0.8660254037844387076, 1.000000000000000000, 0.8660254037844387076, 1.000000000000000000, 0.8660254037844387076, 1.000000000000000000, 0.8660254037844387076, 1.000000000000000000, 0.8660254037844387076, 1.000000000000000000, 0.8660254037844387076, 1.000000000000000000, 0.8660254037844387076, 1.000000000000000000, 0.8660254037844387076, 1.000000000000000000, 0.8660254037844387076, 1.000000000000000000, 0.8660254037844387076, 1.000000000000000000, 0.8660254037844387076, 1.000000000000000000, 0.8660254037844387076, 1.000000000000000000, 0.8660254037844387076, 1.000000000000000000, 0.8660254037844387076, 1.000000000000000000, 0.8660254037844387076, 1.000000000000000000, 0.8660254037844387076, 1.000000000000000000, 0.8660254037844387076, 1.000000000000000000, 0.8660254037844387076, 1.000000000000000000, 0.8660254037844387076, 1.000000000000000000, 0.8660254037844387076, 1.000000000000000000, 0.8660254037844387076, 1.000000000000000000, 0.8660254037844387076, 1.000000000000000000, 0.8660254037844387076, 1.000000000000000000, 0.8660254037844387076, 1.000000000000000000, 0.8660254037844387076, 1.000000000000000000, 0.8660254037844387076, 1.000000000000000000, 0.8660254037844387076, 1.000000000000000000, 0.8660254037844387076, 1.000000000000000000, 0.8660254037844387076, 1.000000000000000000, 0.8660254037844387076, 1.000000000000000000, 0.8660254037844387076, 1.000000000000000000, 0.8660254037844387076, 1.000000000000000000, 0.8660254037844387076, 1.000000000000000000, 0.8660254037844387076, 1.000000000000000000, 0.8660254037844387076, 1.000000000000000000, 0.8660254037844387076, 1.000000000000000000, 0.8660254037844387076, 1.000000000000000000, 0.8660254037844387076, 1.000000000000000000, 0.8660254037844387076, 1.000000000000000000, 0.8660254037844387076, 1.000000000000000000, 0.8660254037844387076, 1.000000000000000000, 0.8660254037844387076, 1.000000000000000000, 0.8660254037844387076, 1.000000000000000000, 0.8660254037844387076, 1.000000000000000000, 0.8660254037844387076, 1.000000000000000000, 0.8660254037844387076, 1.000000000000000000, 0.8660254037844387076, 1.000000000000000000, 0.8660254037844387076, 1.000000000000000000, 0.8660254037844387076, 1.000000000000000000, 0.8660254037844387076, 1.000000000000000000, 0.8660254037844387076, 1.000000000000000000, 0.8660254037844387076, 1.000000000000000000, 0.8660254037844387076, 1.000000000000000000, 0.8660254037844387076, 1.000000000000000000, 0.8660254037844387076, 1.000000000000000000, 0.8660254037844387076, 1.000000000000000000, 0.8660254037844387076, 1.000000000000000000, 0.8660254037844387076, 1.000000000000000000, 0.8660254037844387076, 1.000000000000000000, 0.8660254037844387076, 1.000000000000000000, 0.8660254037844387076, 1.000000000000000000, 0.9111405360107203144, 0.9401542295229963209 ) ) 
 REPRESENTATION_ITEM ( '' )  );
#18257 = CARTESIAN_POINT ( 'NONE',  ( -4.000000000000000000, 2.309401076758498483, -0.4999999999999927280 ) ) ;
#18258 = CARTESIAN_POINT ( 'NONE',  ( 85.40000000000000568, -33.50624999877096855, -101.7320508075688679 ) ) ;
#18259 = CARTESIAN_POINT ( 'NONE',  ( 229.5999999999999375, -34.94999999999999574, 99.99999999999998579 ) ) ;
#18260 = ORIENTED_EDGE ( 'NONE', *, *, #11635, .F. ) ;
#18261 = CARTESIAN_POINT ( 'NONE',  ( 229.8435696437499587, -33.44062499938547717, -51.59142580818350154 ) ) ;
#18262 = DIRECTION ( 'NONE',  ( 0.000000000000000000, 0.000000000000000000, -1.000000000000000000 ) ) ;
#18263 = CARTESIAN_POINT ( 'NONE',  ( 235.3564303562499447, -32.24062499938548143, 98.40857419181659793 ) ) ;
#18264 = CARTESIAN_POINT ( 'NONE',  ( 235.5999999999999943, -35.08124999877096428, -51.73205080756900287 ) ) ;
#18265 = CARTESIAN_POINT ( 'NONE',  ( -80.90000000000000568, -33.00000000000000000, -97.40192378864668399 ) ) ;
#18266 = VERTEX_POINT ( 'NONE', #1785 ) ;
#18267 = ORIENTED_EDGE ( 'NONE', *, *, #18566, .T. ) ;
#18268 = CARTESIAN_POINT ( 'NONE',  ( 244.7999999999999545, -32.00000000000000000, -100.0000000000000000 ) ) ;
#18269 = CARTESIAN_POINT ( 'NONE',  ( -82.40000000000000568, -30.00000000000000355, 99.99999999999998579 ) ) ;
#18270 = CARTESIAN_POINT ( 'NONE',  ( 102.9999999999999858, -5.200000000000008171, -100.0000000000000000 ) ) ;
#18271 = ORIENTED_EDGE ( 'NONE', *, *, #12139, .F. ) ;
#18272 = PLANE ( 'NONE',  #7645 ) ;
#18273 = CARTESIAN_POINT ( 'NONE',  ( -85.40000000000000568, -33.95624999877097139, -98.26794919243111792 ) ) ;
#18274 = COLOUR_RGB ( '',0.8941176470588234615, 0.8941176470588234615, 0.8941176470588234615 ) ;
#18275 = CARTESIAN_POINT ( 'NONE',  ( -2.344047193898593395, -3.265465875126480455, -1.054683074273691752E-14 ) ) ;
#18276 = CARTESIAN_POINT ( 'NONE',  ( -83.90000000000000568, -34.42500000000000426, 102.5980762113533018 ) ) ;
#18277 = CARTESIAN_POINT ( 'NONE',  ( -80.90000000000000568, -34.74374999877097281, 102.5980762113533018 ) ) ;
#18278 = LINE ( 'NONE', #5089, #6965 ) ;
#18279 = FACE_OUTER_BOUND ( 'NONE', #9089, .T. ) ;
#18280 = CARTESIAN_POINT ( 'NONE',  ( 0.000000000000000000, 0.000000000000000000, -0.2800830152838844622 ) ) ;
#18281 = CARTESIAN_POINT ( 'NONE',  ( 232.5999999999999375, -34.55624999877095860, -53.00000000000011369 ) ) ;
#18282 = CARTESIAN_POINT ( 'NONE',  ( 233.9782151781249411, -33.89062499938548001, 97.61286128772489690 ) ) ;
#18283 = CARTESIAN_POINT ( 'NONE',  ( 229.8435696437499303, -32.84062499938547575, 99.99999999999998579 ) ) ;
#18284 = VERTEX_POINT ( 'NONE', #7841 ) ;
#18285 = CARTESIAN_POINT ( 'NONE',  ( -81.02178482187500208, -32.24062499938548854, -97.61286128772489690 ) ) ;
#18286 = ORIENTED_EDGE ( 'NONE', *, *, #18668, .F. ) ;
#18287 = CIRCLE ( 'NONE', #820, 10.00000000000000000 ) ;
#18288 = CARTESIAN_POINT ( 'NONE',  ( 117.5000000000000142, 12.69999999999998508, 110.0000000000000142 ) ) ;
#18289 = CARTESIAN_POINT ( 'NONE',  ( 1.655952806101427033, -3.662737355149048302, -1.182683869819604841E-14 ) ) ;
#18290 = CARTESIAN_POINT ( 'NONE',  ( 4.000000000000000000, 0.9868501483902631932, -0.09357334158579604100 ) ) ;
#18291 = EDGE_LOOP ( 'NONE', ( #1906, #18381, #17060, #16977, #12585 ) ) ;
#18292 = CARTESIAN_POINT ( 'NONE',  ( 232.5999999999999375, -34.07812499938548001, -46.81714838363331666 ) ) ;
#18293 = ORIENTED_EDGE ( 'NONE', *, *, #1728, .T. ) ;
#18294 = ORIENTED_EDGE ( 'NONE', *, *, #6132, .F. ) ;
#18295 = CARTESIAN_POINT ( 'NONE',  ( 81.59615242270662350, -34.57634618820329564, 103.0000000000000000 ) ) ;
#18296 = CARTESIAN_POINT ( 'NONE',  ( 85.15643035625001289, -34.64062499938548711, -99.99999999999998579 ) ) ;
#18297 = MECHANICAL_DESIGN_GEOMETRIC_PRESENTATION_REPRESENTATION (  '', ( #6133 ), #11732 ) ;
#18298 = CARTESIAN_POINT ( 'NONE',  ( -82.39999999999999147, -34.55624999877096570, 96.53589838486223584 ) ) ;
#18299 = CARTESIAN_POINT ( 'NONE',  ( 82.40000000000001990, -32.13750000000000284, -103.0000000000000000 ) ) ;
#18300 = CARTESIAN_POINT ( 'NONE',  ( 82.39999999999999147, -33.20624999877097849, 102.9999999999999858 ) ) ;
#18301 = VECTOR ( 'NONE', #18835, 1000.000000000000000 ) ;
#18302 = CARTESIAN_POINT ( 'NONE',  ( 83.77821517812500929, -33.92812499938548854, -97.61286128772489690 ) ) ;
#18303 = CARTESIAN_POINT ( 'NONE',  ( 82.40000000000001990, -33.26250000000000284, -97.00000000000000000 ) ) ;
#18304 = CARTESIAN_POINT ( 'NONE',  ( -79.64356964374999848, -33.06562499938548427, 99.99999999999998579 ) ) ;
#18305 = CARTESIAN_POINT ( 'NONE',  ( 83.77821517812500929, -34.71562499938548285, -97.61286128772489690 ) ) ;
#18306 = ORIENTED_EDGE ( 'NONE', *, *, #14051, .T. ) ;
#18307 = CARTESIAN_POINT ( 'NONE',  ( 235.5999999999999943, -32.51249999999998863, -48.26794919243124582 ) ) ;
#18308 = SURFACE_STYLE_USAGE ( .BOTH. , #5122 ) ;
#18309 = ADVANCED_FACE ( 'NONE', ( #7748 ), #13705, .F. ) ;
#18310 = EDGE_CURVE ( 'NONE', #10782, #12847, #10486, .T. ) ;
#18311 = CARTESIAN_POINT ( 'NONE',  ( 5.100000000000002309, 0.000000000000000000, 0.000000000000000000 ) ) ;
#18312 = CARTESIAN_POINT ( 'NONE',  ( 229.8435696437499587, -32.99062499938548143, 98.40857419181659793 ) ) ;
#18313 = CARTESIAN_POINT ( 'NONE',  ( -82.39999999999999147, -32.39062499938548001, 103.1828516163667899 ) ) ;
#18314 = CARTESIAN_POINT ( 'NONE',  ( 231.2217848218749339, -32.87812499938547717, -47.61286128772501769 ) ) ;
#18315 = CARTESIAN_POINT ( 'NONE',  ( -79.39999999999999147, -31.98750000000000071, 98.26794919243110371 ) ) ;
#18316 = ORIENTED_EDGE ( 'NONE', *, *, #175, .T. ) ;
#18317 = CARTESIAN_POINT ( 'NONE',  ( -85.31192385480822793, -35.00000000000001421, 99.60674545265970892 ) ) ;
#18318 = CARTESIAN_POINT ( 'NONE',  ( -80.90000000000000568, -33.75000000000000000, -102.5980762113533018 ) ) ;
#18319 = CARTESIAN_POINT ( 'NONE',  ( -81.59615242270662350, -32.38259618943233420, 96.99999999999998579 ) ) ;
#18320 = COLOUR_RGB ( '',0.8941176470588234615, 0.8941176470588234615, 0.8941176470588234615 ) ;
#18321 = EDGE_CURVE ( 'NONE', #2879, #7789, #15105, .T. ) ;
#18322 = CARTESIAN_POINT ( 'NONE',  ( 230.4677467024383475, -31.99999999999998579, -51.75590051601145092 ) ) ;
#18323 = ADVANCED_FACE ( 'NONE', ( #14279 ), #2362, .F. ) ;
#18324 = CARTESIAN_POINT ( 'NONE',  ( -81.02178482187500208, -30.40312499938548640, 97.61286128772489690 ) ) ;
#18325 = AXIS2_PLACEMENT_3D ( 'NONE', #7913, #14157, #9372 ) ;
#18326 = CARTESIAN_POINT ( 'NONE',  ( 80.24533121543018410, -31.99999999999996447, 97.95829548583768087 ) ) ;
#18327 = CARTESIAN_POINT ( 'NONE',  ( 83.77821517812500929, -30.21562499938548285, 102.3871387122750889 ) ) ;
#18328 = B_SPLINE_CURVE_WITH_KNOTS ( 'NONE', 3,
 ( #4452, #11870, #261, #11776, #17935 ),
 .UNSPECIFIED., .F., .F.,
 ( 4, 1, 4 ),
 ( 0.000000000000000000, 0.002309401076758506657, 0.004618802153517013315 ),
 .UNSPECIFIED. ) ;
#18329 = CARTESIAN_POINT ( 'NONE',  ( 81.02178482187500208, -32.35312499938548569, -102.3871387122750889 ) ) ;
#18330 = CARTESIAN_POINT ( 'NONE',  ( 234.0999999999999375, -32.99999999999999289, -47.40192378864679768 ) ) ;
#18331 = CARTESIAN_POINT ( 'NONE',  ( -85.15643035625001289, -34.71562499938548285, 101.5914258081833879 ) ) ;
#18332 = CARTESIAN_POINT ( 'NONE',  ( -82.39999999999999147, -34.41562499938547859, -103.1828516163667899 ) ) ;
#18333 = ORIENTED_EDGE ( 'NONE', *, *, #7762, .T. ) ;
#18334 = CARTESIAN_POINT ( 'NONE',  ( 83.77821517812500929, -31.67812499938548498, 102.3871387122750889 ) ) ;
#18335 =( NAMED_UNIT ( * ) SI_UNIT ( $, .STERADIAN. ) SOLID_ANGLE_UNIT ( ) );
#18336 = CARTESIAN_POINT ( 'NONE',  ( -85.15643035625001289, -33.85312499938549280, 99.99999999999998579 ) ) ;
#18337 = CARTESIAN_POINT ( 'NONE',  ( 232.5999999999999375, -33.48749999999999716, 103.0000000000000000 ) ) ;
#18338 = ORIENTED_EDGE ( 'NONE', *, *, #1500, .F. ) ;
#18339 = CARTESIAN_POINT ( 'NONE',  ( -79.39999999999999147, -31.12500000000000355, -99.99999999999998579 ) ) ;
#18340 = VECTOR ( 'NONE', #167, 1000.000000000000000 ) ;
#18341 = DIRECTION ( 'NONE',  ( 1.000000000000000000, -0.000000000000000000, -0.000000000000000000 ) ) ;
#18342 = CARTESIAN_POINT ( 'NONE',  ( -3.861362476283256129, -2.629030857716004199, -3.671615880910374941 ) ) ;
#18343 = FACE_OUTER_BOUND ( 'NONE', #10097, .T. ) ;
#18344 = PLANE ( 'NONE',  #3635 ) ;
#18345 = CARTESIAN_POINT ( 'NONE',  ( 233.9782151781249411, -33.10312499938547859, 97.61286128772489690 ) ) ;
#18346 = CARTESIAN_POINT ( 'NONE',  ( -83.90000000000000568, -33.92268749875866973, 102.5980762113533018 ) ) ;
#18347 = EDGE_LOOP ( 'NONE', ( #593, #4884, #16529, #16438 ) ) ;
#18348 = LINE ( 'NONE', #4971, #18988 ) ;
#18349 = CARTESIAN_POINT ( 'NONE',  ( 232.5999999999999375, -32.75624999877096144, -53.00000000000010658 ) ) ;
#18350 = CARTESIAN_POINT ( 'NONE',  ( -85.40000000000000568, -33.11250000000000426, 101.7320508075688821 ) ) ;
#18351 = DIRECTION ( 'NONE',  ( -0.000000000000000000, -0.000000000000000000, -1.000000000000000000 ) ) ;
#18352 = PLANE ( 'NONE',  #6154 ) ;
#18353 = CARTESIAN_POINT ( 'NONE',  ( 81.02178482187500208, -32.35312499938548569, -102.3871387122750889 ) ) ;
#18354 = CARTESIAN_POINT ( 'NONE',  ( 111.0000000000000000, 10.19999999999997620, -139.9999999999999716 ) ) ;
#18355 = VECTOR ( 'NONE', #1090, 1000.000000000000114 ) ;
#18356 = ORIENTED_EDGE ( 'NONE', *, *, #11272, .F. ) ;
#18357 = CARTESIAN_POINT ( 'NONE',  ( 235.3564303562499163, -34.98839802032724577, -49.56403331587380023 ) ) ;
#18358 = ITEM_DEFINED_TRANSFORMATION ( 'NONE', 'NONE', #215,  #10540 ) ;
#18359 = CARTESIAN_POINT ( 'NONE',  ( 231.2217848218749339, -32.12812499938547717, 97.61286128772489690 ) ) ;
#18360 = CARTESIAN_POINT ( 'NONE',  ( 229.8435696437499871, -31.64062499938547290, -51.59142580818350865 ) ) ;
#18361 = CARTESIAN_POINT ( 'NONE',  ( -83.77821517812500929, -34.11562499938548854, 102.3871387122750889 ) ) ;
#18362 = CARTESIAN_POINT ( 'NONE',  ( -85.40000000000000568, -34.91250000000000142, 101.7320508075688821 ) ) ;
#18363 = AXIS2_PLACEMENT_3D ( 'NONE', #13068, #6733, #17373 ) ;
#18364 = ORIENTED_EDGE ( 'NONE', *, *, #4224, .T. ) ;
#18366 = ORIENTED_EDGE ( 'NONE', *, *, #14324, .F. ) ;
#18365 = EDGE_CURVE ( 'NONE', #13374, #5491, #17127, .T. ) ;
#18367 = CARTESIAN_POINT ( 'NONE',  ( 4.165266963751927065, 2.049631966911918735, -3.550066703508781174 ) ) ;
#18368 = DIRECTION ( 'NONE',  ( 0.000000000000000000, 0.000000000000000000, -1.000000000000000000 ) ) ;
#18369 = FACE_OUTER_BOUND ( 'NONE', #8666, .T. ) ;
#18370 = ORIENTED_EDGE ( 'NONE', *, *, #8175, .T. ) ;
#18371 = LINE ( 'NONE', #13855, #9516 ) ;
#18372 = CARTESIAN_POINT ( 'NONE',  ( -85.40000000000000568, -32.60624999877097707, -98.26794919243111792 ) ) ;
#18373 = AXIS2_PLACEMENT_3D ( 'NONE', #12241, #9304, #1882 ) ;
#18374 =( BOUNDED_SURFACE ( )  B_SPLINE_SURFACE ( 1, 2, ( 
 ( #8061, #7960, #9523, #7668, #13724, #4949, #15099, #15190, #15489, #5136, #3270, #12268, #365, #10891, #9226, #6314, #12548, #13914, #4849, #18232, #10983, #12362, #16859, #1903, #552, #18519, #6510, #7865, #14016, #13624, #652, #16574, #16756, #3174, #3464, #16952, #9134, #18421, #3564, #1714, #12168, #3372, #18136, #4756, #10699, #9324, #13816, #459, #13034, #17342, #8159, #3663, #6700, #2198, #1032, #3952, #9720, #15879, #15778, #12644, #6895, #5340, #6985, #14108, #12844, #745, #17246, #18813, #17442, #15686, #2290, #8254, #5527, #11081, #2387, #8441, #17148, #18618, #841, #14204, #4053, #5437, #6804, #10012, #9627, #11376, #18719, #5236, #9917, #12750, #15589, #15970, #11185, #2483, #12936, #3755, #1118, #11278, #3853, #9816, #8349, #18908, #14303, #14394, #939, #14487, #11475, #2576, #8537, #7078, #19005, #17051, #4245, #11666, #51, #4341, #11855, #7556, #6002, #1219, #10393, #7363, #2871, #13421, #13320, #19296, #16355, #16452, #10303, #10202, #5909, #17823, #4435, #16261, #16166, #11571, #17630 ),
 ( #10489, #2777, #14588, #8828, #14785, #8630, #2965, #8920, #11952, #5810, #13513, #7175, #14882, #17922, #8730, #14684, #16065, #1319, #3062, #1512, #4531, #2670, #7267, #7461, #4149, #13222, #9024, #5625, #19194, #11760, #17734, #14983, #1411, #1607, #17534, #10110, #13125, #19095, #5716, #9308, #1886, #4833, #12343, #15470, #16843, #18213, #10966, #10588, #12437, #16936, #12150, #3546, #7844, #13894, #9502, #15368, #9404, #6387, #18405, #244, #8037, #2080, #3449, #1984, #5025, #13799, #150, #18307, #16553, #12049, #15077, #3152, #7942, #4927, #18118, #10872, #10774, #1696, #15271, #13708, #532, #9115, #442, #7648, #6295, #6485, #6101, #18025, #4638, #13603, #6203, #4732, #10677, #16738, #16647, #3248, #9206, #15171, #1788, #3348, #7753, #348, #12246, #15759, #5318, #5215, #633, #730, #15950, #11163, #12730, #2367, #17322, #823, #18502, #14376, #11457, #3931, #9897, #3642, #6683, #2551, #14186, #6968, #12626, #6781, #18599, #1012, #18789, #12919, #4034, #11061, #17223, #14283, #920, #8138, #5510 ) ),
 .UNSPECIFIED., .F., .F., .F. ) 
 B_SPLINE_SURFACE_WITH_KNOTS ( ( 2, 2 ),
 ( 3, 2, 2, 2, 2, 2, 2, 2, 2, 2, 2, 2, 2, 2, 2, 2, 2, 2, 2, 2, 2, 2, 2, 2, 2, 2, 2, 2, 2, 2, 2, 2, 2, 2, 2, 2, 2, 2, 2, 2, 2, 2, 2, 2, 2, 2, 2, 2, 2, 2, 2, 2, 2, 2, 2, 2, 2, 2, 2, 2, 2, 2, 2, 2, 2, 2, 2, 2, 3 ),
 ( 0.000000000000000000, 1.000000000000000000 ),
 ( 0.000000000000000000, 0.01388888888888888812, 0.02777777777777777624, 0.04166666666666666435, 0.05555555555555555247, 0.06944444444444444753, 0.08333333333333332871, 0.09722222222222222376, 0.1111111111111111049, 0.1250000000000000000, 0.1388888888888888951, 0.1527777777777777901, 0.1666666666666666574, 0.1805555555555555525, 0.1944444444444444475, 0.2083333333333333426, 0.2222222222222222099, 0.2361111111111111049, 0.2500000000000000000, 0.2638888888888888951, 0.2777777777777777901, 0.2916666666666666852, 0.3055555555555555802, 0.3194444444444444198, 0.3333333333333333148, 0.3472222222222222099, 0.3611111111111111049, 0.3750000000000000000, 0.3888888888888888951, 0.4027777777777777901, 0.4166666666666666852, 0.4305555555555555802, 0.4444444444444444198, 0.4583333333333333148, 0.4722222222222222099, 0.4861111111111111049, 0.5000000000000000000, 0.5138888888888888395, 0.5277777777777777901, 0.5416666666666666297, 0.5555555555555555802, 0.5694444444444444198, 0.5833333333333333703, 0.5972222222222222099, 0.6111111111111111605, 0.6250000000000000000, 0.6388888888888888395, 0.6527777777777777901, 0.6666666666666666297, 0.6805555555555555802, 0.6944444444444444198, 0.7083333333333333703, 0.7222222222222222099, 0.7361111111111111605, 0.7500000000000000000, 0.7638888888888888395, 0.7777777777777777901, 0.7916666666666666297, 0.8055555555555555802, 0.8194444444444444198, 0.8333333333333333703, 0.8472222222222222099, 0.8611111111111111605, 0.8750000000000000000, 0.8888888888888888395, 0.9027777777777777901, 0.9166666666666666297, 0.9258785066912882389, 0.9351372917582011501 ),
 .UNSPECIFIED. ) 
 GEOMETRIC_REPRESENTATION_ITEM ( )  RATIONAL_B_SPLINE_SURFACE ( (
 ( 1.000000000000000000, 0.8660254037844387076, 1.000000000000000000, 0.8660254037844387076, 1.000000000000000000, 0.8660254037844387076, 1.000000000000000000, 0.8660254037844387076, 1.000000000000000000, 0.8660254037844387076, 1.000000000000000000, 0.8660254037844387076, 1.000000000000000000, 0.8660254037844387076, 1.000000000000000000, 0.8660254037844387076, 1.000000000000000000, 0.8660254037844387076, 1.000000000000000000, 0.8660254037844387076, 1.000000000000000000, 0.8660254037844387076, 1.000000000000000000, 0.8660254037844387076, 1.000000000000000000, 0.8660254037844387076, 1.000000000000000000, 0.8660254037844387076, 1.000000000000000000, 0.8660254037844387076, 1.000000000000000000, 0.8660254037844387076, 1.000000000000000000, 0.8660254037844387076, 1.000000000000000000, 0.8660254037844387076, 1.000000000000000000, 0.8660254037844387076, 1.000000000000000000, 0.8660254037844387076, 1.000000000000000000, 0.8660254037844387076, 1.000000000000000000, 0.8660254037844387076, 1.000000000000000000, 0.8660254037844387076, 1.000000000000000000, 0.8660254037844387076, 1.000000000000000000, 0.8660254037844387076, 1.000000000000000000, 0.8660254037844387076, 1.000000000000000000, 0.8660254037844387076, 1.000000000000000000, 0.8660254037844387076, 1.000000000000000000, 0.8660254037844387076, 1.000000000000000000, 0.8660254037844387076, 1.000000000000000000, 0.8660254037844387076, 1.000000000000000000, 0.8660254037844387076, 1.000000000000000000, 0.8660254037844387076, 1.000000000000000000, 0.8660254037844387076, 1.000000000000000000, 0.8660254037844387076, 1.000000000000000000, 0.8660254037844387076, 1.000000000000000000, 0.8660254037844387076, 1.000000000000000000, 0.8660254037844387076, 1.000000000000000000, 0.8660254037844387076, 1.000000000000000000, 0.8660254037844387076, 1.000000000000000000, 0.8660254037844387076, 1.000000000000000000, 0.8660254037844387076, 1.000000000000000000, 0.8660254037844387076, 1.000000000000000000, 0.8660254037844387076, 1.000000000000000000, 0.8660254037844387076, 1.000000000000000000, 0.8660254037844387076, 1.000000000000000000, 0.8660254037844387076, 1.000000000000000000, 0.8660254037844387076, 1.000000000000000000, 0.8660254037844387076, 1.000000000000000000, 0.8660254037844387076, 1.000000000000000000, 0.8660254037844387076, 1.000000000000000000, 0.8660254037844387076, 1.000000000000000000, 0.8660254037844387076, 1.000000000000000000, 0.8660254037844387076, 1.000000000000000000, 0.8660254037844387076, 1.000000000000000000, 0.8660254037844387076, 1.000000000000000000, 0.8660254037844387076, 1.000000000000000000, 0.8660254037844387076, 1.000000000000000000, 0.8660254037844387076, 1.000000000000000000, 0.8660254037844387076, 1.000000000000000000, 0.8660254037844387076, 1.000000000000000000, 0.8660254037844387076, 1.000000000000000000, 0.8660254037844387076, 1.000000000000000000, 0.8660254037844387076, 1.000000000000000000, 0.8660254037844387076, 1.000000000000000000, 0.8660254037844387076, 1.000000000000000000, 0.9111410165655264848, 0.9401539157124900736, 0.9401539157124900736, 0.9401539157124900736),
 ( 1.000000000000000000, 0.8660254037844387076, 1.000000000000000000, 0.8660254037844387076, 1.000000000000000000, 0.8660254037844387076, 1.000000000000000000, 0.8660254037844387076, 1.000000000000000000, 0.8660254037844387076, 1.000000000000000000, 0.8660254037844387076, 1.000000000000000000, 0.8660254037844387076, 1.000000000000000000, 0.8660254037844387076, 1.000000000000000000, 0.8660254037844387076, 1.000000000000000000, 0.8660254037844387076, 1.000000000000000000, 0.8660254037844387076, 1.000000000000000000, 0.8660254037844387076, 1.000000000000000000, 0.8660254037844387076, 1.000000000000000000, 0.8660254037844387076, 1.000000000000000000, 0.8660254037844387076, 1.000000000000000000, 0.8660254037844387076, 1.000000000000000000, 0.8660254037844387076, 1.000000000000000000, 0.8660254037844387076, 1.000000000000000000, 0.8660254037844387076, 1.000000000000000000, 0.8660254037844387076, 1.000000000000000000, 0.8660254037844387076, 1.000000000000000000, 0.8660254037844387076, 1.000000000000000000, 0.8660254037844387076, 1.000000000000000000, 0.8660254037844387076, 1.000000000000000000, 0.8660254037844387076, 1.000000000000000000, 0.8660254037844387076, 1.000000000000000000, 0.8660254037844387076, 1.000000000000000000, 0.8660254037844387076, 1.000000000000000000, 0.8660254037844387076, 1.000000000000000000, 0.8660254037844387076, 1.000000000000000000, 0.8660254037844387076, 1.000000000000000000, 0.8660254037844387076, 1.000000000000000000, 0.8660254037844387076, 1.000000000000000000, 0.8660254037844387076, 1.000000000000000000, 0.8660254037844387076, 1.000000000000000000, 0.8660254037844387076, 1.000000000000000000, 0.8660254037844387076, 1.000000000000000000, 0.8660254037844387076, 1.000000000000000000, 0.8660254037844387076, 1.000000000000000000, 0.8660254037844387076, 1.000000000000000000, 0.8660254037844387076, 1.000000000000000000, 0.8660254037844387076, 1.000000000000000000, 0.8660254037844387076, 1.000000000000000000, 0.8660254037844387076, 1.000000000000000000, 0.8660254037844387076, 1.000000000000000000, 0.8660254037844387076, 1.000000000000000000, 0.8660254037844387076, 1.000000000000000000, 0.8660254037844387076, 1.000000000000000000, 0.8660254037844387076, 1.000000000000000000, 0.8660254037844387076, 1.000000000000000000, 0.8660254037844387076, 1.000000000000000000, 0.8660254037844387076, 1.000000000000000000, 0.8660254037844387076, 1.000000000000000000, 0.8660254037844387076, 1.000000000000000000, 0.8660254037844387076, 1.000000000000000000, 0.8660254037844387076, 1.000000000000000000, 0.8660254037844387076, 1.000000000000000000, 0.8660254037844387076, 1.000000000000000000, 0.8660254037844387076, 1.000000000000000000, 0.8660254037844387076, 1.000000000000000000, 0.8660254037844387076, 1.000000000000000000, 0.8660254037844387076, 1.000000000000000000, 0.8660254037844387076, 1.000000000000000000, 0.8660254037844387076, 1.000000000000000000, 0.8660254037844387076, 1.000000000000000000, 0.8660254037844387076, 1.000000000000000000, 0.9111410165655264848, 0.9401539157124900736, 0.9401539157124900736, 0.9401539157124900736) ) ) 
 REPRESENTATION_ITEM ( '' )  SURFACE ( )  );
#18375 = CARTESIAN_POINT ( 'NONE',  ( -85.15643035625001289, -35.22676544108147567, 98.99674642581742035 ) ) ;
#18376 = CARTESIAN_POINT ( 'NONE',  ( -82.39999999999999147, -31.18124999877096926, 103.4641016151377499 ) ) ;
#18377 = CARTESIAN_POINT ( 'NONE',  ( -83.90000000000000568, -33.61874999877097281, 97.40192378864668399 ) ) ;
#18378 = DIRECTION ( 'NONE',  ( 1.000000000000000000, 0.000000000000000000, 0.000000000000000000 ) ) ;
#18379 = DIRECTION ( 'NONE',  ( 0.000000000000000000, -1.000000000000000000, 0.000000000000000000 ) ) ;
#18380 = CARTESIAN_POINT ( 'NONE',  ( 231.2217848218749339, -34.11562499938548143, 102.3871387122750889 ) ) ;
#18381 = ORIENTED_EDGE ( 'NONE', *, *, #18571, .T. ) ;
#18382 = SURFACE_STYLE_USAGE ( .BOTH. , #9090 ) ;
#18383 = CARTESIAN_POINT ( 'NONE',  ( 235.5999999999999943, -31.03124999877096357, 98.26794919243110371 ) ) ;
#18384 = CARTESIAN_POINT ( 'NONE',  ( 4.170895651974601215, 4.109780709045311120, -8.452559493485846499E-14 ) ) ;
#18385 = ORIENTED_EDGE ( 'NONE', *, *, #6183, .T. ) ;
#18386 = DIRECTION ( 'NONE',  ( -0.000000000000000000, 0.000000000000000000, -1.000000000000000000 ) ) ;
#18387 = CARTESIAN_POINT ( 'NONE',  ( 1.216174376970875689E-15, -2.686816014504582739, -2.346298152288355698 ) ) ;
#18388 = UNCERTAINTY_MEASURE_WITH_UNIT (LENGTH_MEASURE( 1.000000000000000082E-05 ), #5002, 'distance_accuracy_value', 'NONE');
#18389 = CARTESIAN_POINT ( 'NONE',  ( 229.7688980899055196, -35.00000000000000000, -50.85751801881856693 ) ) ;
#18390 = ORIENTED_EDGE ( 'NONE', *, *, #8766, .T. ) ;
#18391 = CARTESIAN_POINT ( 'NONE',  ( 231.2217848218749339, -34.56562499938547717, -47.61286128772501769 ) ) ;
#18392 = ORIENTED_EDGE ( 'NONE', *, *, #14393, .T. ) ;
#18393 = ORIENTED_EDGE ( 'NONE', *, *, #7168, .F. ) ;
#18394 = CARTESIAN_POINT ( 'NONE',  ( 234.0999999999999375, -33.44999999999999574, -47.40192378864679768 ) ) ;
#18395 = CARTESIAN_POINT ( 'NONE',  ( 79.39999999999999147, -31.57499999999999929, -99.99999999999998579 ) ) ;
#18396 = CARTESIAN_POINT ( 'NONE',  ( -79.64356964374999848, -34.97812499938548569, -99.99999999999998579 ) ) ;
#18397 = CARTESIAN_POINT ( 'NONE',  ( -80.90000000000000568, -34.14374999877097139, 97.40192378864668399 ) ) ;
#18398 = LINE ( 'NONE', #5312, #16625 ) ;
#18399 = CARTESIAN_POINT ( 'NONE',  ( 81.02178482187500208, -32.65312499938548996, -97.61286128772489690 ) ) ;
#18400 = ADVANCED_FACE ( 'NONE', ( #14182 ), #915, .T. ) ;
#18401 = DIRECTION ( 'NONE',  ( 1.000000000000000000, 0.000000000000000000, -0.000000000000000000 ) ) ;
#18402 = CARTESIAN_POINT ( 'NONE',  ( -79.64356964374999848, -32.16562499938548569, 99.99999999999998579 ) ) ;
#18403 = CARTESIAN_POINT ( 'NONE',  ( 82.39999999999999147, -33.62812499938549138, -103.1828516163667899 ) ) ;
#18404 = ORIENTED_EDGE ( 'NONE', *, *, #11156, .T. ) ;
#18405 = CARTESIAN_POINT ( 'NONE',  ( 231.0999999999999375, -32.17499999999999716, -47.40192378864679768 ) ) ;
#18406 = CARTESIAN_POINT ( 'NONE',  ( -82.39999999999999147, -33.48750000000000426, 103.4641016151377499 ) ) ;
#18407 = CARTESIAN_POINT ( 'NONE',  ( 79.68596062386910717, -31.99999999999998579, -101.2782762865714972 ) ) ;
#18408 = CARTESIAN_POINT ( 'NONE',  ( 231.2217848218749339, -32.12812499938547717, 97.61286128772489690 ) ) ;
#18409 = CARTESIAN_POINT ( 'NONE',  ( -82.39999999999999147, -30.59062499938548640, 103.1828516163667899 ) ) ;
#18410 = CARTESIAN_POINT ( 'NONE',  ( 229.8435696437499871, -32.54062499938547859, -51.59142580818350865 ) ) ;
#18411 = CARTESIAN_POINT ( 'NONE',  ( -85.40000000000000568, -32.70000000000000284, 99.99999999999998579 ) ) ;
#18412 = VERTEX_POINT ( 'NONE', #629 ) ;
#18413 = DIRECTION ( 'NONE',  ( 1.000000000000000000, -1.387778780781445676E-15, -2.407412430484046130E-31 ) ) ;
#18414 = CARTESIAN_POINT ( 'NONE',  ( 4.175813232069148562, 4.122719923832742772, -5.545971589517866732E-16 ) ) ;
#18415 = CARTESIAN_POINT ( 'NONE',  ( 83.77821517812500929, -31.41562499938548569, 97.61286128772489690 ) ) ;
#18416 = CARTESIAN_POINT ( 'NONE',  ( 85.14613134194621580, -32.00000000000003553, -99.70214005991869044 ) ) ;
#18417 = CARTESIAN_POINT ( 'NONE',  ( -83.77821517812500929, -31.67812499938548498, 97.61286128772489690 ) ) ;
#18418 = CARTESIAN_POINT ( 'NONE',  ( 82.15584532983334043, -31.99999999999999289, 97.13032736203115292 ) ) ;
#18419 = CARTESIAN_POINT ( 'NONE',  ( 85.15643035625001289, -34.30312499938548854, 99.99999999999998579 ) ) ;
#18420 = CARTESIAN_POINT ( 'NONE',  ( 85.15643035625001289, -31.60312499938548569, -99.99999999999998579 ) ) ;
#18421 = CARTESIAN_POINT ( 'NONE',  ( 229.8435696437499871, -31.52812499938547575, -51.59142580818350865 ) ) ;
#18422 = CARTESIAN_POINT ( 'NONE',  ( -79.77811200999887831, -35.00000000000000000, 100.8506536761481414 ) ) ;
#18423 = CARTESIAN_POINT ( 'NONE',  ( -79.64356964375001269, -32.76562499938548711, -98.40857419181659793 ) ) ;
#18424 = ORIENTED_EDGE ( 'NONE', *, *, #7530, .T. ) ;
#18425 = APPLICATION_CONTEXT ( 'automotive_design' ) ;
#18426 = CARTESIAN_POINT ( 'NONE',  ( 82.39999999999999147, -32.39062499938548001, 96.81714838363319586 ) ) ;
#18427 = CARTESIAN_POINT ( 'NONE',  ( 4.030867648404662162, -3.732851566701945067, -0.5345114293593726806 ) ) ;
#18428 = CARTESIAN_POINT ( 'NONE',  ( -85.15643035624999868, -30.55312499938548854, 101.5914258081833879 ) ) ;
#18429 = EDGE_CURVE ( 'NONE', #19060, #4909, #10374, .T. ) ;
#18430 = CARTESIAN_POINT ( 'NONE',  ( -83.77821517812500929, -33.02812499938548285, 97.61286128772489690 ) ) ;
#18431 = EDGE_CURVE ( 'NONE', #13374, #13408, #18594, .T. ) ;
#18432 = CARTESIAN_POINT ( 'NONE',  ( 110.0000000000000000, 10.19999999999997620, -137.3499999999999943 ) ) ;
#18433 = VERTEX_POINT ( 'NONE', #8418 ) ;
#18434 = CARTESIAN_POINT ( 'NONE',  ( -85.40000000000000568, -33.11250000000000426, -98.26794919243111792 ) ) ;
#18435 = CARTESIAN_POINT ( 'NONE',  ( -6.473970235329672780E-16, -4.862606272033106691, -3.745885042887442395 ) ) ;
#18436 = CARTESIAN_POINT ( 'NONE',  ( 82.65333140691205926, -34.99995246259152282, -97.01071553687880566 ) ) ;
#18437 = CARTESIAN_POINT ( 'NONE',  ( -96.99999999999998579, 0.000000000000000000, -150.0000000000000000 ) ) ;
#18438 = EDGE_CURVE ( 'NONE', #7254, #15345, #15659, .T. ) ;
#18439 = CARTESIAN_POINT ( 'NONE',  ( 229.8435696437499303, -35.20312499938548001, 99.99999999999998579 ) ) ;
#18440 = CARTESIAN_POINT ( 'NONE',  ( -79.39999999999999147, -33.28518749875868110, 98.26794919243110371 ) ) ;
#18441 = ORIENTED_EDGE ( 'NONE', *, *, #5204, .T. ) ;
#18442 = CARTESIAN_POINT ( 'NONE',  ( -85.15643035625001289, -35.22676544108147567, 98.99674642581742035 ) ) ;
#18443 = CARTESIAN_POINT ( 'NONE',  ( -85.40000000000000568, -33.58124999877097139, -101.7320508075688821 ) ) ;
#18444 = DIRECTION ( 'NONE',  ( -0.000000000000000000, -1.000000000000000000, -0.000000000000000000 ) ) ;
#18445 = UNCERTAINTY_MEASURE_WITH_UNIT (LENGTH_MEASURE( 1.000000000000000082E-05 ), #14859, 'distance_accuracy_value', 'NONE');
#18446 = CARTESIAN_POINT ( 'NONE',  ( -85.40000000000000568, -34.48124999877096997, 98.26794919243111792 ) ) ;
#18447 = CARTESIAN_POINT ( 'NONE',  ( 83.77821517812500929, -31.07812499938548711, -102.3871387122750889 ) ) ;
#18448 = CARTESIAN_POINT ( 'NONE',  ( 82.40000000000000568, -30.00000000000000355, -99.99999999999998579 ) ) ;
#18449 = ORIENTED_EDGE ( 'NONE', *, *, #7478, .T. ) ;
#18450 = CARTESIAN_POINT ( 'NONE',  ( 79.39999999999999147, -31.48124999877097352, 101.7320508075688821 ) ) ;
#18451 = SHAPE_DEFINITION_REPRESENTATION ( #8581, #19222 ) ;
#18452 = CARTESIAN_POINT ( 'NONE',  ( 229.8435696437499303, -32.95312499938548001, 99.99999999999998579 ) ) ;
#18453 = CARTESIAN_POINT ( 'NONE',  ( 229.8435696437499871, -31.11562499938547788, -48.40857419181671162 ) ) ;
#18454 = ADVANCED_FACE ( 'NONE', ( #14372 ), #11808, .F. ) ;
#18455 = CARTESIAN_POINT ( 'NONE',  ( -79.64356964374999848, -33.96562499938548285, 99.99999999999998579 ) ) ;
#18456 = CARTESIAN_POINT ( 'NONE',  ( 82.39999999999999147, -33.20624999877097849, 103.0000000000000000 ) ) ;
#18457 = ORIENTED_EDGE ( 'NONE', *, *, #11033, .T. ) ;
#18458 = ORIENTED_EDGE ( 'NONE', *, *, #4260, .T. ) ;
#18459 = CARTESIAN_POINT ( 'NONE',  ( -83.77821517812500929, -32.01562499938548001, -102.3871387122750889 ) ) ;
#18460 = EDGE_CURVE ( 'NONE', #5869, #104, #12060, .T. ) ;
#18461 = FACE_OUTER_BOUND ( 'NONE', #13466, .T. ) ;
#18462 = CARTESIAN_POINT ( 'NONE',  ( 232.5999999999999375, -34.55624999877095860, 97.00000000000000000 ) ) ;
#18463 = ORIENTED_EDGE ( 'NONE', *, *, #8045, .T. ) ;
#18464 = CARTESIAN_POINT ( 'NONE',  ( -82.40000000000000568, -50.00000000000000000, 99.99999999999998579 ) ) ;
#18465 = CARTESIAN_POINT ( 'NONE',  ( -82.39999999999999147, -33.88124999877096855, -96.53589838486223584 ) ) ;
#18466 = CARTESIAN_POINT ( 'NONE',  ( -82.41196654184768988, -35.00000000000001421, 97.00083539721711645 ) ) ;
#18467 = CARTESIAN_POINT ( 'NONE',  ( -79.39999999999999147, -32.45624999877097139, 101.7320508075688537 ) ) ;
#18468 = CARTESIAN_POINT ( 'NONE',  ( -79.39999999999999147, -34.70624999877097139, 101.7320508075688537 ) ) ;
#18469 = CARTESIAN_POINT ( 'NONE',  ( -82.40000000000001990, -32.13750000000000284, 103.0000000000000000 ) ) ;
#18470 = EDGE_CURVE ( 'NONE', #17768, #779, #5117, .T. ) ;
#18471 = CARTESIAN_POINT ( 'NONE',  ( 244.7999999999999545, -32.00000000000001421, -103.0000000000000142 ) ) ;
#18472 = CARTESIAN_POINT ( 'NONE',  ( 229.8435696437499871, -33.32812499938548001, 98.40857419181659793 ) ) ;
#18473 = ORIENTED_EDGE ( 'NONE', *, *, #6395, .T. ) ;
#18474 = CARTESIAN_POINT ( 'NONE',  ( 231.0999999999999375, -30.76874999877096428, 102.5980762113533018 ) ) ;
#18475 = CARTESIAN_POINT ( 'NONE',  ( -81.59615242270662350, -32.96115380933864003, -97.00000000000000000 ) ) ;
#18476 = ORIENTED_EDGE ( 'NONE', *, *, #2657, .T. ) ;
#18477 = CARTESIAN_POINT ( 'NONE',  ( -79.39999999999999147, -33.41250000000000142, -98.26794919243113213 ) ) ;
#18478 = CARTESIAN_POINT ( 'NONE',  ( 244.7999999999999545, -35.00000000000002842, 147.7999999999999829 ) ) ;
#18479 = CARTESIAN_POINT ( 'NONE',  ( 3.355112389629172576, -2.681727112203168950, -0.2256878752776777242 ) ) ;
#18480 = ORIENTED_EDGE ( 'NONE', *, *, #12618, .F. ) ;
#18481 = CARTESIAN_POINT ( 'NONE',  ( -85.40000000000000568, -33.95624999877097139, -98.26794919243111792 ) ) ;
#18482 = AXIS2_PLACEMENT_3D ( 'NONE', #541, #18413, #158 ) ;
#18483 =( BOUNDED_CURVE ( )  B_SPLINE_CURVE ( 2, ( #3736, #12824, #5415, #3830, #9701, #8328, #17032, #17422, #6583 ),
 .UNSPECIFIED., .F., .F. ) 
 B_SPLINE_CURVE_WITH_KNOTS ( ( 3, 2, 2, 2, 3 ),
 ( 0.5208333333333333703, 0.5277777777777777901, 0.5416666666666666297, 0.5555555555555555802, 0.5625000000000000000 ),
 .UNSPECIFIED. ) 
 CURVE ( )  GEOMETRIC_REPRESENTATION_ITEM ( )  RATIONAL_B_SPLINE_CURVE ( ( 0.9330127018922192983, 0.9330127018922198534, 1.000000000000000000, 0.8660254037844387076, 1.000000000000000000, 0.8660254037844387076, 1.000000000000000000, 0.9330127018922194093, 0.9330127018922194093 ) ) 
 REPRESENTATION_ITEM ( '' )  );
#18484 = AXIS2_PLACEMENT_3D ( 'NONE', #18678, #17108, #6949 ) ;
#18485 = CARTESIAN_POINT ( 'NONE',  ( 233.4038475772933339, -33.86115380933863150, -47.00000000000012790 ) ) ;
#18486 = ORIENTED_EDGE ( 'NONE', *, *, #1511, .T. ) ;
#18487 = LINE ( 'NONE', #18108, #14759 ) ;
#18488 = CARTESIAN_POINT ( 'NONE',  ( 83.90000000000000568, -30.82500000000000284, -102.5980762113533018 ) ) ;
#18489 = ADVANCED_FACE ( 'NONE', ( #7241 ), #13010, .F. ) ;
#18490 = DIRECTION ( 'NONE',  ( -0.000000000000000000, -1.000000000000000000, -0.000000000000000000 ) ) ;
#18491 = CARTESIAN_POINT ( 'NONE',  ( -83.90000000000000568, -33.61874999877097281, 97.40192378864668399 ) ) ;
#18492 = CARTESIAN_POINT ( 'NONE',  ( -85.40000000000000568, -34.90856250001228744, 101.7320508075688679 ) ) ;
#18493 = CARTESIAN_POINT ( 'NONE',  ( -81.59615242270662350, -33.22634618820330843, 97.00000000000000000 ) ) ;
#18494 = FILL_AREA_STYLE_COLOUR ( '', #11627 ) ;
#18495 = CARTESIAN_POINT ( 'NONE',  ( 83.77821517812500929, -32.12812499938548427, -97.61286128772489690 ) ) ;
#18496 = CARTESIAN_POINT ( 'NONE',  ( 4.071447262713888016, -2.020725942163695166, -3.500000000000000000 ) ) ;
#18497 = CARTESIAN_POINT ( 'NONE',  ( -79.64356964375001269, -33.92812499938548854, 98.40857419181659793 ) ) ;
#18498 = VECTOR ( 'NONE', #14954, 1000.000000000000000 ) ;
#18499 = AXIS2_PLACEMENT_3D ( 'NONE', #15078, #12050, #7649 ) ;
#18500 = CARTESIAN_POINT ( 'NONE',  ( 83.77821517812500929, -34.11562499938548854, -102.3871387122750889 ) ) ;
#18501 = ORIENTED_EDGE ( 'NONE', *, *, #11072, .F. ) ;
#18502 = CARTESIAN_POINT ( 'NONE',  ( 235.5999999999999375, -34.27499999999999147, -50.00000000000011369 ) ) ;
#18503 = FILL_AREA_STYLE ('',( #16844 ) ) ;
#18504 = CARTESIAN_POINT ( 'NONE',  ( 83.20384757729335945, -33.63615380933863008, -96.99999999999998579 ) ) ;
#18505 = CARTESIAN_POINT ( 'NONE',  ( 83.90000000000000568, -33.52499999999999858, 97.40192378864668399 ) ) ;
#18506 = CARTESIAN_POINT ( 'NONE',  ( -83.77821517812500929, -31.67812499938548498, 97.61286128772489690 ) ) ;
#18507 = CARTESIAN_POINT ( 'NONE',  ( 231.2217848218749339, -32.12812499938547717, -52.38713871227520968 ) ) ;
#18508 = CARTESIAN_POINT ( 'NONE',  ( -83.90000000000000568, -32.62500000000000000, 102.5980762113533018 ) ) ;
#18509 = ORIENTED_EDGE ( 'NONE', *, *, #4830, .T. ) ;
#18510 = CARTESIAN_POINT ( 'NONE',  ( 3.880214671983734043, -0.7309020039786090495, 3.500000000000000444 ) ) ;
#18511 = CIRCLE ( 'NONE', #2281, 5.199999999999996625 ) ;
#18512 = CARTESIAN_POINT ( 'NONE',  ( 79.83361526238431338, -35.00000000000000000, 98.97827398863964277 ) ) ;
#18513 = CARTESIAN_POINT ( 'NONE',  ( 79.64356964374999848, -33.06562499938548427, 99.99999999999998579 ) ) ;
#18514 = CARTESIAN_POINT ( 'NONE',  ( 80.90000000000000568, -32.10000000000000142, -102.5980762113533018 ) ) ;
#18515 = CARTESIAN_POINT ( 'NONE',  ( -85.15643035625001289, -31.60312499938548569, 99.99999999999998579 ) ) ;
#18516 = CARTESIAN_POINT ( 'NONE',  ( -79.64356964374998427, -32.76562499938548711, -98.40857419181659793 ) ) ;
#18517 = CARTESIAN_POINT ( 'NONE',  ( 81.02178482187500208, -31.19062499938548427, 102.3871387122750889 ) ) ;
#18518 = CARTESIAN_POINT ( 'NONE',  ( 85.15643035624999868, -32.09062499938548996, -98.40857419181659793 ) ) ;
#18519 = CARTESIAN_POINT ( 'NONE',  ( 229.8435696437499871, -31.07812499938548001, -51.59142580818350865 ) ) ;
#18520 = CARTESIAN_POINT ( 'NONE',  ( -79.64356964374998427, -34.94062499938548427, 98.40857419181659793 ) ) ;
#18521 = CARTESIAN_POINT ( 'NONE',  ( -79.64356964375001269, -34.49062499938548854, -101.5914258081833879 ) ) ;
#18522 = EDGE_LOOP ( 'NONE', ( #4517, #14145, #1983 ) ) ;
#18523 = CARTESIAN_POINT ( 'NONE',  ( 79.64356964375001269, -32.31562499938548427, 98.40857419181659793 ) ) ;
#18524 = CARTESIAN_POINT ( 'NONE',  ( 232.5999999999999375, -33.88124999877096855, -47.00000000000011369 ) ) ;
#18525 = CARTESIAN_POINT ( 'NONE',  ( 105.1999999999999744, -34.99999999999999289, -100.0000000000000000 ) ) ;
#18526 = CARTESIAN_POINT ( 'NONE',  ( -79.64356964374999848, -33.62812499938548427, 99.99999999999998579 ) ) ;
#18527 =( BOUNDED_SURFACE ( )  B_SPLINE_SURFACE ( 3, 2, ( 
 ( #17034, #9608, #2184 ),
 ( #3738, #8239, #12921 ),
 ( #2650, #8614, #7058 ),
 ( #18892, #18794, #3832 ),
 ( #1100, #12827, #4225 ),
 ( #8712, #11649, #10181 ) ),
 .UNSPECIFIED., .F., .F., .F. ) 
 B_SPLINE_SURFACE_WITH_KNOTS ( ( 4, 2, 4 ),
 ( 3, 3 ),
 ( 0.02032853247518125531, 0.02278863295364820865, 0.02524873343211516200 ),
 ( 0.000000000000000000, 1.000000000000000000 ),
 .UNSPECIFIED. ) 
 GEOMETRIC_REPRESENTATION_ITEM ( )  RATIONAL_B_SPLINE_SURFACE ( (
 ( 1.000000000000000000, 0.8047781615896836271, 1.000000000000000000),
 ( 1.000000000000000000, 0.8123767586289967202, 1.000000000000000000),
 ( 1.000000000000000000, 0.8190662415563443322, 1.000000000000000000),
 ( 1.000000000000000000, 0.8192361015669982205, 1.000000000000000000),
 ( 1.000000000000000000, 0.8126135807103181952, 1.000000000000000000),
 ( 1.000000000000000000, 0.8047712338318587788, 1.000000000000000000) ) ) 
 REPRESENTATION_ITEM ( '' )  SURFACE ( )  );
#18528 = DIRECTION ( 'NONE',  ( -1.000000000000000000, -0.000000000000000000, -0.000000000000000000 ) ) ;
#18529 = EDGE_LOOP ( 'NONE', ( #11624, #17944, #13442, #9186, #1061, #13657 ) ) ;
#18530 = CARTESIAN_POINT ( 'NONE',  ( -82.39999999999999147, -34.38750000000000284, -96.53589838486223584 ) ) ;
#18531 = DIRECTION ( 'NONE',  ( 0.000000000000000000, -1.000000000000000000, 0.000000000000000000 ) ) ;
#18532 = DIRECTION ( 'NONE',  ( -0.000000000000000000, 0.000000000000000000, -1.000000000000000000 ) ) ;
#18533 = CARTESIAN_POINT ( 'NONE',  ( -84.51155386534844638, -35.25364837475780888, -101.7717924772919957 ) ) ;
#18534 = CARTESIAN_POINT ( 'NONE',  ( 229.8435696437499871, -33.89062499938548001, 98.40857419181659793 ) ) ;
#18535 = CARTESIAN_POINT ( 'NONE',  ( -82.39999999999999147, -33.88518749875868252, 103.4641016151377499 ) ) ;
#18536 = VERTEX_POINT ( 'NONE', #1294 ) ;
#18537 = CARTESIAN_POINT ( 'NONE',  ( -81.02178482187500208, -34.90312499938548285, 97.61286128772489690 ) ) ;
#18538 = DIRECTION ( 'NONE',  ( 0.000000000000000000, -1.000000000000000000, 0.000000000000000000 ) ) ;
#18539 = CARTESIAN_POINT ( 'NONE',  ( 85.15643035625001289, -34.67812499938548143, 101.5914258081833879 ) ) ;
#18540 = CARTESIAN_POINT ( 'NONE',  ( -94.79999999999999716, 0.000000000000000000, -150.0000000000000000 ) ) ;
#18541 = DIRECTION ( 'NONE',  ( -1.000000000000000000, -0.000000000000000000, -0.000000000000000000 ) ) ;
#18542 = CARTESIAN_POINT ( 'NONE',  ( 79.64356964375001269, -31.41562499938548569, -101.5914258081833879 ) ) ;
#18543 = CYLINDRICAL_SURFACE ( 'NONE', #13962, 6.000000000000015987 ) ;
#18544 = EDGE_CURVE ( 'NONE', #17308, #5485, #13196, .T. ) ;
#18545 = ORIENTED_EDGE ( 'NONE', *, *, #1956, .F. ) ;
#18546 = APPLICATION_PROTOCOL_DEFINITION ( 'draft international standard', 'automotive_design', 1998, #14194 ) ;
#18547 = CARTESIAN_POINT ( 'NONE',  ( 229.8435696437499871, -32.09062499938548285, 98.40857419181659793 ) ) ;
#18548 = CARTESIAN_POINT ( 'NONE',  ( 235.3564303562499447, -34.07812499938548001, -50.00000000000011369 ) ) ;
#18549 = ADVANCED_FACE ( 'NONE', ( #19169 ), #5591, .T. ) ;
#18550 = EDGE_CURVE ( 'NONE', #8999, #15031, #11452, .T. ) ;
#18551 = CARTESIAN_POINT ( 'NONE',  ( -85.15643035624999868, -32.35312499938549280, 101.5914258081833879 ) ) ;
#18552 = DIRECTION ( 'NONE',  ( 1.000000000000000000, -1.586032892321652482E-15, -0.000000000000000000 ) ) ;
#18553 = ORIENTED_EDGE ( 'NONE', *, *, #13543, .T. ) ;
#18554 = EDGE_LOOP ( 'NONE', ( #4496, #9558, #335, #8195, #5120, #5145, #9511 ) ) ;
#18555 = CARTESIAN_POINT ( 'NONE',  ( -82.39999999999999147, -30.47812499938548569, -96.81714838363319586 ) ) ;
#18556 = CARTESIAN_POINT ( 'NONE',  ( -85.40000000000000568, -32.21250000000000568, -98.26794919243111792 ) ) ;
#18557 = ORIENTED_EDGE ( 'NONE', *, *, #18571, .F. ) ;
#18558 = CARTESIAN_POINT ( 'NONE',  ( 81.02178482187500208, -32.35312499938548569, 97.61286128772489690 ) ) ;
#18559 = CARTESIAN_POINT ( 'NONE',  ( -85.40000000000000568, -34.85624999877096997, -98.26794919243111792 ) ) ;
#18560 = CARTESIAN_POINT ( 'NONE',  ( 82.39999999999999147, -34.83749999999999858, 96.53589838486223584 ) ) ;
#18561 = CARTESIAN_POINT ( 'NONE',  ( -82.39999999999999147, -31.91249999999999787, 96.99999999999998579 ) ) ;
#18562 = CARTESIAN_POINT ( 'NONE',  ( -79.39999999999999147, -31.55624999877096926, 101.7320508075688537 ) ) ;
#18563 = CARTESIAN_POINT ( 'NONE',  ( -79.39999999999999147, -34.18124999877097281, 98.26794919243110371 ) ) ;
#18564 = CARTESIAN_POINT ( 'NONE',  ( -85.40000000000000568, -32.21250000000000568, 101.7320508075688821 ) ) ;
#18565 = PRODUCT_DEFINITION_SHAPE ( 'NONE', 'NONE',  #14653 ) ;
#18566 = EDGE_CURVE ( 'NONE', #4877, #10357, #600, .T. ) ;
#18567 = CARTESIAN_POINT ( 'NONE',  ( 80.90000000000000568, -34.29374999877096997, -102.5980762113533018 ) ) ;
#18568 = EDGE_CURVE ( 'NONE', #19033, #7323, #19064, .T. ) ;
#18569 = CARTESIAN_POINT ( 'NONE',  ( 110.0000000000000142, 15.19999999999997797, -150.0000000000000000 ) ) ;
#18570 = CARTESIAN_POINT ( 'NONE',  ( 233.9782151781249411, -34.34062499938547575, 97.61286128772489690 ) ) ;
#18571 = EDGE_CURVE ( 'NONE', #15250, #4279, #1586, .T. ) ;
#18572 = ORIENTED_EDGE ( 'NONE', *, *, #11276, .F. ) ;
#18573 = APPLICATION_CONTEXT ( 'automotive_design' ) ;
#18574 = CARTESIAN_POINT ( 'NONE',  ( 82.39999999999999147, -32.50312499938548427, -96.81714838363319586 ) ) ;
#18575 = CARTESIAN_POINT ( 'NONE',  ( 231.0999999999999375, -31.36874999877096215, 97.40192378864668399 ) ) ;
#18576 = CARTESIAN_POINT ( 'NONE',  ( 232.5999999999999375, -32.30624999877096570, 97.00000000000000000 ) ) ;
#18577 = EDGE_LOOP ( 'NONE', ( #5739, #5842, #8597, #13082 ) ) ;
#18578 = ADVANCED_BREP_SHAPE_REPRESENTATION ( '', ( #9467, #10540 ), #9915 ) ;
#18579 = CARTESIAN_POINT ( 'NONE',  ( -85.40000000000000568, -33.58124999877097139, 98.26794919243111792 ) ) ;
#18580 = CARTESIAN_POINT ( 'NONE',  ( 110.0000000000000142, 15.19999999999997797, -145.0000000000000000 ) ) ;
#18581 = CARTESIAN_POINT ( 'NONE',  ( 5.599999999999998757, 0.000000000000000000, 0.000000000000000000 ) ) ;
#18582 = ORIENTED_EDGE ( 'NONE', *, *, #18005, .F. ) ;
#18583 = CARTESIAN_POINT ( 'NONE',  ( 112.2864669432758831, 9.160276915580404022, -133.9627822341408034 ) ) ;
#18584 = CARTESIAN_POINT ( 'NONE',  ( 4.211140560182196957, -2.431303136016555122, -3.745885042887436622 ) ) ;
#18585 = ORIENTED_EDGE ( 'NONE', *, *, #8205, .F. ) ;
#18586 = CARTESIAN_POINT ( 'NONE',  ( -82.40000000000001990, -32.13750000000000284, -97.00000000000000000 ) ) ;
#18587 = CARTESIAN_POINT ( 'NONE',  ( 80.90000000000000568, -30.60000000000000142, -97.40192378864668399 ) ) ;
#18588 = CYLINDRICAL_SURFACE ( 'NONE', #4555, 3.000000000000002665 ) ;
#18589 = CARTESIAN_POINT ( 'NONE',  ( -79.39999999999999147, -34.63124999877096855, 98.26794919243110371 ) ) ;
#18590 = CARTESIAN_POINT ( 'NONE',  ( -80.90000000000000568, -33.74606250001229313, 97.40192378864668399 ) ) ;
#18591 = CARTESIAN_POINT ( 'NONE',  ( 105.1999999999999744, -31.99999999999999289, 150.0000000000000000 ) ) ;
#18592 = SURFACE_STYLE_FILL_AREA ( #2175 ) ;
#18593 = CARTESIAN_POINT ( 'NONE',  ( 85.40000000000000568, -33.95624999877097139, 98.26794919243111792 ) ) ;
#18594 = LINE ( 'NONE', #8323, #9303 ) ;
#18595 = CARTESIAN_POINT ( 'NONE',  ( -83.77821517812500929, -32.91562499938547859, 97.61286128772489690 ) ) ;
#18596 = AXIS2_PLACEMENT_3D ( 'NONE', #1045, #1333, #19017 ) ;
#18597 = CARTESIAN_POINT ( 'NONE',  ( -84.70388354820684640, -35.00002705695768412, 98.07851859032987818 ) ) ;
#18598 = VERTEX_POINT ( 'NONE', #7152 ) ;
#18599 = CARTESIAN_POINT ( 'NONE',  ( 235.5999999999999375, -34.72499999999999432, -50.00000000000011369 ) ) ;
#18600 = EDGE_CURVE ( 'NONE', #6642, #6725, #8325, .T. ) ;
#18601 = CARTESIAN_POINT ( 'NONE',  ( -83.90000000000000568, -34.87500000000000000, 102.5980762113533018 ) ) ;
#18602 =( BOUNDED_CURVE ( )  B_SPLINE_CURVE ( 2, ( #15483, #12164, #10887, #12356, #18324, #7767, #13619, #262, #15094, #13720, #454, #1803, #2095, #6309, #5037, #16661, #1998, #3368, #17046, #3459, #10789, #9130, #361, #15185, #12263, #5132, #6505, #7861, #647, #6217, #8056, #6596, #18228, #12544, #16855, #3560, #18515, #10979, #18417, #15385, #14011, #11077, #1709, #3265, #9320, #4942, #4844, #7955, #16948, #9418, #9519, #9221, #18131, #15284, #7664, #4751, #10695, #16750, #1899, #13909, #13813, #6403, #546, #12450, #740, #9812, #11370, #10008, #8250, #14200, #2286, #17438, #3657, #8343, #1028, #9716, #6696, #12746, #6799, #15964, #5523, #12640, #13029, #6890, #18614, #18713, #14389, #837, #19001, #2571, #14104, #8533, #15774, #14482, #5336, #5621, #11273, #5231, #1114, #17337, #11180, #6980, #17242, #11567, #7071, #17144, #9623, #2382, #15584, #3846, #2194, #14299, #5433, #3947, #9912, #935, #12840, #8152, #15680, #18808, #15875, #12932, #3750, #2479, #8437, #18902, #11471, #4049, #1215, #216, #10650, #6268, #17728, #414, #8727 ),
 .UNSPECIFIED., .F., .F. ) 
 B_SPLINE_CURVE_WITH_KNOTS ( ( 3, 2, 2, 2, 2, 2, 2, 2, 2, 2, 2, 2, 2, 2, 2, 2, 2, 2, 2, 2, 2, 2, 2, 2, 2, 2, 2, 2, 2, 2, 2, 2, 2, 2, 2, 2, 2, 2, 2, 2, 2, 2, 2, 2, 2, 2, 2, 2, 2, 2, 2, 2, 2, 2, 2, 2, 2, 2, 2, 2, 2, 2, 2, 2, 2, 2, 2, 3 ),
 ( 0.000000000000000000, 0.01500076810536658638, 0.03000153621073317275, 0.04500230431609975740, 0.06000307242146634551, 0.07500384052683294056, 0.09000460863219951479, 0.1050053767375661029, 0.1200061448429326910, 0.1350069129482992791, 0.1500076810536658811, 0.1650084491590324554, 0.1800092172643990296, 0.1950099853697656316, 0.2100107534751322058, 0.2250115215804988078, 0.2400122896858653820, 0.2550130577912319563, 0.2700138258965985583, 0.2850145940019651603, 0.3000153621073317622, 0.3150161302126983087, 0.3300168983180649107, 0.3450176664234314572, 0.3600184345287980592, 0.3750192026341646612, 0.3900199707395312632, 0.4050207388448978096, 0.4200215069502644116, 0.4350222750556310136, 0.4500230431609976156, 0.4650238112663642176, 0.4800245793717307641, 0.4950253474770973106, 0.5100261155824639125, 0.5250268836878305700, 0.5400276517931971165, 0.5550284198985636630, 0.5700291880039303205, 0.5850299561092968670, 0.6000307242146635245, 0.6150314923200299599, 0.6300322604253966174, 0.6450330285307631639, 0.6600337966361298214, 0.6750345647414963679, 0.6900353328468629144, 0.7050361009522295719, 0.7200368690575961184, 0.7350376371629627759, 0.7500384052683293223, 0.7650391733736959798, 0.7800399414790625263, 0.7950407095844291838, 0.8100414776897956193, 0.8250422457951621658, 0.8400430139005288233, 0.8550437820058953697, 0.8700445501112620272, 0.8850453182166285737, 0.9000460863219952312, 0.9150468544273617777, 0.9300476225327284352, 0.9450483906380949817, 0.9600491587434615282, 0.9750499268488280746, 0.9900506949541946211, 1.000000000000000000 ),
 .UNSPECIFIED. ) 
 CURVE ( )  GEOMETRIC_REPRESENTATION_ITEM ( )  RATIONAL_B_SPLINE_CURVE ( ( 1.000000000000000000, 0.8660254037844387076, 1.000000000000000000, 0.8660254037844387076, 1.000000000000000000, 0.8660254037844387076, 1.000000000000000000, 0.8660254037844387076, 1.000000000000000000, 0.8660254037844387076, 1.000000000000000000, 0.8660254037844387076, 1.000000000000000000, 0.8660254037844387076, 1.000000000000000000, 0.8660254037844387076, 1.000000000000000000, 0.8660254037844387076, 1.000000000000000000, 0.8660254037844387076, 1.000000000000000000, 0.8660254037844387076, 1.000000000000000000, 0.8660254037844387076, 1.000000000000000000, 0.8660254037844387076, 1.000000000000000000, 0.8660254037844387076, 1.000000000000000000, 0.8660254037844387076, 1.000000000000000000, 0.8660254037844387076, 1.000000000000000000, 0.8660254037844387076, 1.000000000000000000, 0.8660254037844387076, 1.000000000000000000, 0.8660254037844387076, 1.000000000000000000, 0.8660254037844387076, 1.000000000000000000, 0.8660254037844387076, 1.000000000000000000, 0.8660254037844387076, 1.000000000000000000, 0.8660254037844387076, 1.000000000000000000, 0.8660254037844387076, 1.000000000000000000, 0.8660254037844387076, 1.000000000000000000, 0.8660254037844387076, 1.000000000000000000, 0.8660254037844387076, 1.000000000000000000, 0.8660254037844387076, 1.000000000000000000, 0.8660254037844387076, 1.000000000000000000, 0.8660254037844387076, 1.000000000000000000, 0.8660254037844387076, 1.000000000000000000, 0.8660254037844387076, 1.000000000000000000, 0.8660254037844387076, 1.000000000000000000, 0.8660254037844387076, 1.000000000000000000, 0.8660254037844387076, 1.000000000000000000, 0.8660254037844387076, 1.000000000000000000, 0.8660254037844387076, 1.000000000000000000, 0.8660254037844387076, 1.000000000000000000, 0.8660254037844387076, 1.000000000000000000, 0.8660254037844387076, 1.000000000000000000, 0.8660254037844387076, 1.000000000000000000, 0.8660254037844387076, 1.000000000000000000, 0.8660254037844387076, 1.000000000000000000, 0.8660254037844387076, 1.000000000000000000, 0.8660254037844387076, 1.000000000000000000, 0.8660254037844387076, 1.000000000000000000, 0.8660254037844387076, 1.000000000000000000, 0.8660254037844387076, 1.000000000000000000, 0.8660254037844387076, 1.000000000000000000, 0.8660254037844387076, 1.000000000000000000, 0.8660254037844387076, 1.000000000000000000, 0.8660254037844387076, 1.000000000000000000, 0.8660254037844387076, 1.000000000000000000, 0.8660254037844387076, 1.000000000000000000, 0.8660254037844387076, 1.000000000000000000, 0.8660254037844387076, 1.000000000000000000, 0.8660254037844387076, 1.000000000000000000, 0.8660254037844387076, 1.000000000000000000, 0.8660254037844387076, 1.000000000000000000, 0.8660254037844387076, 1.000000000000000000, 0.8660254037844387076, 1.000000000000000000, 0.8660254037844387076, 1.000000000000000000, 0.8660254037844387076, 1.000000000000000000, 0.8660254037844387076, 1.000000000000000000, 0.8660254037844387076, 1.000000000000000000, 0.8660254037844387076, 1.000000000000000000, 0.9111409417988175496, 0.9401539645359766606 ) ) 
 REPRESENTATION_ITEM ( '' )  );
#18603 = LINE ( 'NONE', #15571, #2631 ) ;
#18604 = CARTESIAN_POINT ( 'NONE',  ( 235.3564303562499447, -32.24062499938548143, 98.40857419181659793 ) ) ;
#18605 = CARTESIAN_POINT ( 'NONE',  ( -81.02178482187500208, -34.00312499938548427, 97.61286128772489690 ) ) ;
#18606 = CARTESIAN_POINT ( 'NONE',  ( 229.8435696437499871, -35.16562499938547148, -48.40857419181671162 ) ) ;
#18607 = VERTEX_POINT ( 'NONE', #4030 ) ;
#18608 = CARTESIAN_POINT ( 'NONE',  ( 3.948095570617042860, 0.6965071952231317587, 3.500000000000155875 ) ) ;
#18609 = ADVANCED_FACE ( 'NONE', ( #11832 ), #17853, .F. ) ;
#18610 = CIRCLE ( 'NONE', #1127, 2.100000000000000089 ) ;
#18611 = CARTESIAN_POINT ( 'NONE',  ( -82.40000000000000568, -34.78124999877096712, 102.9999999999999858 ) ) ;
#18612 = CARTESIAN_POINT ( 'NONE',  ( 81.02178482187500208, -31.79062499938548925, 97.61286128772489690 ) ) ;
#18613 = CARTESIAN_POINT ( 'NONE',  ( 2.000000000000008882, 3.464101615137749945, 0.000000000000000000 ) ) ;
#18614 = CARTESIAN_POINT ( 'NONE',  ( -85.15643035625001289, -33.40312499938548285, 99.99999999999998579 ) ) ;
#18615 = CARTESIAN_POINT ( 'NONE',  ( 83.74167325096738068, -32.00000000000000000, 97.53412486788937485 ) ) ;
#18616 = CARTESIAN_POINT ( 'NONE',  ( 82.39999999999999147, -31.82812499938548356, 96.81714838363319586 ) ) ;
#18617 = CARTESIAN_POINT ( 'NONE',  ( 85.15643035625001289, -32.95312499938548711, -99.99999999999998579 ) ) ;
#18618 = CARTESIAN_POINT ( 'NONE',  ( 235.3564303562499447, -33.02812499938547575, -51.59142580818350865 ) ) ;
#18619 = CARTESIAN_POINT ( 'NONE',  ( -85.15643035625001289, -33.89062499938548711, 98.40857419181659793 ) ) ;
#18620 = CARTESIAN_POINT ( 'NONE',  ( -82.39999999999999147, -31.60312499938548569, -103.1828516163667899 ) ) ;
#18621 = ORIENTED_EDGE ( 'NONE', *, *, #16631, .T. ) ;
#18622 = CARTESIAN_POINT ( 'NONE',  ( 83.77821517812500929, -31.97812499938548925, 97.61286128772489690 ) ) ;
#18623 = CARTESIAN_POINT ( 'NONE',  ( 4.158921614371310582, -4.076055977742311320, 0.05993604794450450857 ) ) ;
#18624 = CARTESIAN_POINT ( 'NONE',  ( -82.39999999999999147, -34.16250000000000142, 96.53589838486223584 ) ) ;
#18625 = CARTESIAN_POINT ( 'NONE',  ( -81.02178482187500208, -31.64062499938548356, 97.61286128772489690 ) ) ;
#18626 = CARTESIAN_POINT ( 'NONE',  ( -85.15643035624999868, -33.89062499938548711, 98.40857419181659793 ) ) ;
#18627 = DIRECTION ( 'NONE',  ( 0.000000000000000000, -1.000000000000000000, 0.000000000000000000 ) ) ;
#18628 = ORIENTED_EDGE ( 'NONE', *, *, #8869, .F. ) ;
#18629 = CARTESIAN_POINT ( 'NONE',  ( -80.90000000000000568, -33.00000000000000000, -97.40192378864668399 ) ) ;
#18630 = CARTESIAN_POINT ( 'NONE',  ( -79.64356964375001269, -31.86562499938548143, -98.40857419181659793 ) ) ;
#18631 = CARTESIAN_POINT ( 'NONE',  ( 80.90000000000000568, -32.85000000000000142, -97.40192378864668399 ) ) ;
#18632 = CARTESIAN_POINT ( 'NONE',  ( 84.42750213138106119, -35.00000000000000000, -97.77995849557630947 ) ) ;
#18633 = CARTESIAN_POINT ( 'NONE',  ( 235.3564303562499447, -30.85312499938547859, 101.5914258081833879 ) ) ;
#18634 = CARTESIAN_POINT ( 'NONE',  ( -83.90000000000000568, -34.97268749875867400, 97.40192378864668399 ) ) ;
#18635 = CARTESIAN_POINT ( 'NONE',  ( -83.90000000000000568, -34.81874999877096855, 102.5980762113533018 ) ) ;
#18636 = CARTESIAN_POINT ( 'NONE',  ( 110.0000000000000142, 10.19999999999997620, -150.0000000000000000 ) ) ;
#18637 = CARTESIAN_POINT ( 'NONE',  ( -83.90000000000000568, -33.16874999877096286, -102.5980762113533018 ) ) ;
#18638 = DIRECTION ( 'NONE',  ( 1.000000000000000000, 3.548298019043479384E-15, 0.000000000000000000 ) ) ;
#18639 = VECTOR ( 'NONE', #11742, 1000.000000000000000 ) ;
#18640 = CARTESIAN_POINT ( 'NONE',  ( 231.7961524227065695, -34.80134618820329706, -47.00000000000011369 ) ) ;
#18641 = CARTESIAN_POINT ( 'NONE',  ( 81.02178482187500208, -31.45312499938549067, -102.3871387122750889 ) ) ;
#18642 = CARTESIAN_POINT ( 'NONE',  ( 4.175326769692871309, 2.060699556488903461, 3.569236330973477145 ) ) ;
#18643 = EDGE_LOOP ( 'NONE', ( #18222, #37, #3979, #8540, #13114, #4637 ) ) ;
#18644 =( BOUNDED_CURVE ( )  B_SPLINE_CURVE ( 2, ( #11619, #8782, #5862, #11815, #15926, #2528, #16313, #1174, #4391 ),
 .UNSPECIFIED., .F., .F. ) 
 B_SPLINE_CURVE_WITH_KNOTS ( ( 3, 2, 2, 2, 3 ),
 ( 0.7708333333333332593, 0.7777777777777777901, 0.7916666666666666297, 0.8055555555555555802, 0.8125000000000000000 ),
 .UNSPECIFIED. ) 
 CURVE ( )  GEOMETRIC_REPRESENTATION_ITEM ( )  RATIONAL_B_SPLINE_CURVE ( ( 0.9330127018922192983, 0.9330127018922187432, 1.000000000000000000, 0.8660254037844387076, 1.000000000000000000, 0.8660254037844387076, 1.000000000000000000, 0.9330127018922194093, 0.9330127018922194093 ) ) 
 REPRESENTATION_ITEM ( '' )  );
#18645 = CARTESIAN_POINT ( 'NONE',  ( 80.90000000000000568, -30.54374999877096997, 102.5980762113533018 ) ) ;
#18646 = PRODUCT_CONTEXT ( 'NONE', #4709, 'mechanical' ) ;
#18647 = CARTESIAN_POINT ( 'NONE',  ( 232.5999999999999375, -32.39062499938548001, 103.1828516163667899 ) ) ;
#18648 = CARTESIAN_POINT ( 'NONE',  ( 235.3564303562499447, -32.72812499938547859, -50.00000000000011369 ) ) ;
#18649 = VECTOR ( 'NONE', #9548, 1000.000000000000000 ) ;
#18650 = AXIS2_PLACEMENT_3D ( 'NONE', #168, #10323, #8752 ) ;
#18651 = CARTESIAN_POINT ( 'NONE',  ( -79.64356964375001269, -33.55312499938548854, 101.5914258081833879 ) ) ;
#18652 = FACE_OUTER_BOUND ( 'NONE', #15352, .T. ) ;
#18653 = ORIENTED_EDGE ( 'NONE', *, *, #9586, .T. ) ;
#18654 = EDGE_LOOP ( 'NONE', ( #8334, #16696, #3803, #6349 ) ) ;
#18655 = CARTESIAN_POINT ( 'NONE',  ( -79.64356964374999848, -32.61562499938548854, -99.99999999999998579 ) ) ;
#18656 = CARTESIAN_POINT ( 'NONE',  ( 105.1999999999999744, -4.999999999999976907, 153.0000000000000000 ) ) ;
#18657 = ORIENTED_EDGE ( 'NONE', *, *, #14051, .F. ) ;
#18658 = CARTESIAN_POINT ( 'NONE',  ( 79.64356964374998427, -34.11562499938548854, 98.40857419181659793 ) ) ;
#18659 = CONICAL_SURFACE ( 'NONE', #2747, 4.000000000000000000, 0.8911886515913786111 ) ;
#18660 = CARTESIAN_POINT ( 'NONE',  ( -83.90000000000000568, -33.91874999877096997, -97.40192378864668399 ) ) ;
#18661 = CARTESIAN_POINT ( 'NONE',  ( 80.90000000000000568, -33.89999999999999858, 97.40192378864668399 ) ) ;
#18662 = CARTESIAN_POINT ( 'NONE',  ( 229.8435696437499871, -30.29062499938548214, 98.40857419181659793 ) ) ;
#18663 = CARTESIAN_POINT ( 'NONE',  ( -80.90000000000000568, -32.34374999877096712, 97.40192378864668399 ) ) ;
#18664 = CARTESIAN_POINT ( 'NONE',  ( -79.39999999999999147, -34.63124999877096855, 98.26794919243110371 ) ) ;
#18665 = CIRCLE ( 'NONE', #1800, 5.200000000000009948 ) ;
#18666 = CARTESIAN_POINT ( 'NONE',  ( 84.70388354820684640, -35.00002705695777649, -98.07851859032987818 ) ) ;
#18667 = ADVANCED_FACE ( 'NONE', ( #7819 ), #17994, .F. ) ;
#18668 = EDGE_CURVE ( 'NONE', #14513, #13499, #12022, .T. ) ;
#18669 = CARTESIAN_POINT ( 'NONE',  ( 235.5999999999999943, -32.45624999877096428, 101.7320508075688537 ) ) ;
#18670 = CARTESIAN_POINT ( 'NONE',  ( 231.2583267490322783, -32.00000000000000000, 102.4658751321104120 ) ) ;
#18671 = CARTESIAN_POINT ( 'NONE',  ( 235.3564303562499447, -33.55312499938548143, 101.5914258081833879 ) ) ;
#18672 = ORIENTED_EDGE ( 'NONE', *, *, #11558, .F. ) ;
#18673 = CARTESIAN_POINT ( 'NONE',  ( 79.64356964374998427, -32.12812499938548427, -98.40857419181659793 ) ) ;
#18674 = CARTESIAN_POINT ( 'NONE',  ( 234.0999999999999375, -31.59374999877096712, 102.5980762113533018 ) ) ;
#18675 = CARTESIAN_POINT ( 'NONE',  ( 229.5999999999999375, -31.70624999877096073, -48.26794919243123161 ) ) ;
#18676 = EDGE_LOOP ( 'NONE', ( #16043, #17232, #641, #17367, #1105 ) ) ;
#18677 = CARTESIAN_POINT ( 'NONE',  ( -83.77821517812500929, -31.86562499938548498, 102.3871387122750889 ) ) ;
#18678 = CARTESIAN_POINT ( 'NONE',  ( 232.5999999999999375, -29.99999999999999645, 99.99999999999998579 ) ) ;
#18679 = EDGE_LOOP ( 'NONE', ( #15258, #4889, #14077, #3651, #7276 ) ) ;
#18680 = CARTESIAN_POINT ( 'NONE',  ( 4.052424581287801253, -2.393186648133309724, 2.990837702970520873 ) ) ;
#18681 = AXIS2_PLACEMENT_3D ( 'NONE', #1051, #11302, #19023 ) ;
#18683 = EDGE_CURVE ( 'NONE', #5783, #12300, #3121, .T. ) ;
#18682 = CARTESIAN_POINT ( 'NONE',  ( 4.071447262713887127, -2.020725942163688060, 3.500000000000000444 ) ) ;
#18684 = ORIENTED_EDGE ( 'NONE', *, *, #4701, .T. ) ;
#18685 =( BOUNDED_CURVE ( )  B_SPLINE_CURVE ( 2, ( #14277, #17317, #12819, #18882, #17415, #11451, #723, #11157, #12289, #3291, #1735, #11996, #1557, #13746, #5951, #7792, #1646, #384, #10532, #10815, #12188, #13461, #16397, #18157, #12093, #10433, #3197, #6142, #15216, #16500, #4779, #14933, #6337, #6049, #4480, #13552, #4677, #17869, #16592, #7693, #9251, #15026, #18254, #18066, #3007, #8965, #97, #2, #7504, #1832, #17964, #9156, #10627, #15119, #4574, #11898, #3103, #1453, #9061, #13650, #7599, #192, #13369, #292, #4871, #6241, #10722, #16686, #7406, #16782, #3396, #14555, #3584, #18539, #5358, #6718, #8084, #860, #479, #2308, #6823, #17267, #14127 ),
 .UNSPECIFIED., .F., .F. ) 
 B_SPLINE_CURVE_WITH_KNOTS ( ( 3, 2, 2, 2, 2, 2, 2, 2, 2, 2, 2, 2, 2, 2, 2, 2, 2, 2, 2, 2, 2, 2, 2, 2, 2, 2, 2, 2, 2, 2, 2, 2, 2, 2, 2, 2, 2, 2, 2, 2, 2, 3 ),
 ( 0.3716916592825996735, 0.3750191855951752751, 0.3900199530189822905, 0.4050207204427893615, 0.4200214878665963769, 0.4350222552904033924, 0.4500230227142104078, 0.4650237901380174232, 0.4800245575618243832, 0.4950253249856314541, 0.5100260924094384141, 0.5250268598332454850, 0.5400276272570524450, 0.5550283946808594049, 0.5700291621046664758, 0.5850299295284735468, 0.6000306969522806178, 0.6150314643760875777, 0.6300322317998945376, 0.6450329992237016086, 0.6600337666475086795, 0.6750345340713156395, 0.6900353014951225994, 0.7050360689189296703, 0.7200368363427367413, 0.7350376037665437012, 0.7500383711903506612, 0.7650391386141577321, 0.7800399060379648031, 0.7950406734617718740, 0.8100414408855787229, 0.8250422083093857939, 0.8400429757331928649, 0.8550437431569998248, 0.8700445105808068957, 0.8850452780046138557, 0.9000460454284209266, 0.9150468128522277755, 0.9300475802760350685, 0.9450483476998419174, 0.9600491151236487664, 0.9717223562348824561 ),
 .UNSPECIFIED. ) 
 CURVE ( )  GEOMETRIC_REPRESENTATION_ITEM ( )  RATIONAL_B_SPLINE_CURVE ( ( 0.9537471549766856072, 0.9702812541832720461, 1.000000000000000000, 0.8660254037844387076, 1.000000000000000000, 0.8660254037844387076, 1.000000000000000000, 0.8660254037844387076, 1.000000000000000000, 0.8660254037844387076, 1.000000000000000000, 0.8660254037844387076, 1.000000000000000000, 0.8660254037844387076, 1.000000000000000000, 0.8660254037844387076, 1.000000000000000000, 0.8660254037844387076, 1.000000000000000000, 0.8660254037844387076, 1.000000000000000000, 0.8660254037844387076, 1.000000000000000000, 0.8660254037844387076, 1.000000000000000000, 0.8660254037844387076, 1.000000000000000000, 0.8660254037844387076, 1.000000000000000000, 0.8660254037844387076, 1.000000000000000000, 0.8660254037844387076, 1.000000000000000000, 0.8660254037844387076, 1.000000000000000000, 0.8660254037844387076, 1.000000000000000000, 0.8660254037844387076, 1.000000000000000000, 0.8660254037844387076, 1.000000000000000000, 0.8660254037844387076, 1.000000000000000000, 0.8660254037844387076, 1.000000000000000000, 0.8660254037844387076, 1.000000000000000000, 0.8660254037844387076, 1.000000000000000000, 0.8660254037844387076, 1.000000000000000000, 0.8660254037844387076, 1.000000000000000000, 0.8660254037844387076, 1.000000000000000000, 0.8660254037844387076, 1.000000000000000000, 0.8660254037844387076, 1.000000000000000000, 0.8660254037844387076, 1.000000000000000000, 0.8660254037844387076, 1.000000000000000000, 0.8660254037844387076, 1.000000000000000000, 0.8660254037844387076, 1.000000000000000000, 0.8660254037844387076, 1.000000000000000000, 0.8660254037844387076, 1.000000000000000000, 0.8660254037844387076, 1.000000000000000000, 0.8660254037844387076, 1.000000000000000000, 0.8660254037844387076, 1.000000000000000000, 0.8660254037844387076, 1.000000000000000000, 0.8660254037844387076, 1.000000000000000000, 0.8957441496011472326, 0.9537471549767071455 ) ) 
 REPRESENTATION_ITEM ( '' )  );
#18686 = FILL_AREA_STYLE ('',( #17211 ) ) ;
#18687 = B_SPLINE_CURVE_WITH_KNOTS ( 'NONE', 3,
 ( #18846, #19032, #4082, #9952, #5467 ),
 .UNSPECIFIED., .F., .F.,
 ( 4, 1, 4 ),
 ( 0.000000000000000000, 0.002020725942163690506, 0.004041451884327381880 ),
 .UNSPECIFIED. ) ;
#18688 = CARTESIAN_POINT ( 'NONE',  ( 85.40000000000000568, -32.25000000000000000, -99.99999999999998579 ) ) ;
#18689 = DIRECTION ( 'NONE',  ( 0.000000000000000000, 0.000000000000000000, -1.000000000000000000 ) ) ;
#18690 = B_SPLINE_CURVE_WITH_KNOTS ( 'NONE', 3,
 ( #4801, #5875, #3313, #11826, #13386, #13570 ),
 .UNSPECIFIED., .F., .F.,
 ( 4, 2, 4 ),
 ( 0.000000000000000000, 0.0002095117440864791795, 0.0004190234881729583589 ),
 .UNSPECIFIED. ) ;
#18691 = CARTESIAN_POINT ( 'NONE',  ( -79.39999999999999147, -33.28124999877096712, 98.26794919243110371 ) ) ;
#18692 = CARTESIAN_POINT ( 'NONE',  ( -79.39999999999999147, -30.71250000000000568, 101.7320508075688537 ) ) ;
#18693 = CARTESIAN_POINT ( 'NONE',  ( 85.40000000000000568, -32.25000000000000000, -99.99999999999998579 ) ) ;
#18694 = CARTESIAN_POINT ( 'NONE',  ( 99.99999999999994316, -29.80000000000000782, -150.0000000000000000 ) ) ;
#18695 = EDGE_CURVE ( 'NONE', #15015, #17250, #8068, .T. ) ;
#18696 = CARTESIAN_POINT ( 'NONE',  ( 83.20384757729335945, -34.08615380933863293, 102.9999999999999858 ) ) ;
#18697 = VECTOR ( 'NONE', #15804, 1000.000000000000000 ) ;
#18698 = DIRECTION ( 'NONE',  ( 0.000000000000000000, -1.000000000000000000, 0.000000000000000000 ) ) ;
#18699 = CARTESIAN_POINT ( 'NONE',  ( -85.15643035624999868, -33.77812499938548285, 98.40857419181659793 ) ) ;
#18700 = DIRECTION ( 'NONE',  ( 1.387778780781445676E-15, 1.000000000000000000, 0.000000000000000000 ) ) ;
#18701 = ORIENTED_EDGE ( 'NONE', *, *, #10457, .F. ) ;
#18702 = DIRECTION ( 'NONE',  ( 0.000000000000000000, 1.000000000000000000, 0.000000000000000000 ) ) ;
#18703 = CARTESIAN_POINT ( 'NONE',  ( 233.9782151781249411, -32.80312499938548143, 102.3871387122750889 ) ) ;
#18704 = CARTESIAN_POINT ( 'NONE',  ( -85.15643035624999868, -32.91562499938549280, 101.5914258081833879 ) ) ;
#18705 = CARTESIAN_POINT ( 'NONE',  ( 229.8435696437499871, -30.17812499938547433, -51.59142580818350865 ) ) ;
#18706 = ORIENTED_EDGE ( 'NONE', *, *, #1350, .F. ) ;
#18707 = CARTESIAN_POINT ( 'NONE',  ( -82.65333140691201663, -34.99995246259153703, 97.01071553687880566 ) ) ;
#18708 = CARTESIAN_POINT ( 'NONE',  ( -79.64356964375001269, -33.02812499938548285, 98.40857419181659793 ) ) ;
#18709 = CYLINDRICAL_SURFACE ( 'NONE', #14404, 5.200000000000009948 ) ;
#18710 = CARTESIAN_POINT ( 'NONE',  ( 81.02178482187500208, -33.14062499938548711, 97.61286128772489690 ) ) ;
#18711 = CARTESIAN_POINT ( 'NONE',  ( 229.5999999999999375, -33.13124999877096144, -51.73205080756898866 ) ) ;
#18712 = DIRECTION ( 'NONE',  ( -0.000000000000000000, -1.000000000000000000, 0.000000000000000000 ) ) ;
#18713 = CARTESIAN_POINT ( 'NONE',  ( -85.15643035625001289, -33.44062499938548427, 98.40857419181659793 ) ) ;
#18714 = CARTESIAN_POINT ( 'NONE',  ( -85.15643035625001289, -33.85312499938549280, -99.99999999999998579 ) ) ;
#18715 = CARTESIAN_POINT ( 'NONE',  ( 79.64356964375001269, -33.10312499938549280, 98.40857419181659793 ) ) ;
#18716 =( BOUNDED_CURVE ( )  B_SPLINE_CURVE ( 2, ( #11882, #7585, #17850, #18142, #15104, #7294, #9140, #10515, #1629 ),
 .UNSPECIFIED., .F., .T. ) 
 B_SPLINE_CURVE_WITH_KNOTS ( ( 3, 2, 2, 2, 3 ),
 ( 0.7291666666666666297, 0.7361111111111111605, 0.7500000000000000000, 0.7638888888888888395, 0.7708333333333331483 ),
 .UNSPECIFIED. ) 
 CURVE ( )  GEOMETRIC_REPRESENTATION_ITEM ( )  RATIONAL_B_SPLINE_CURVE ( ( 0.9330127018922192983, 0.9330127018922187432, 1.000000000000000000, 0.8660254037844387076, 1.000000000000000000, 0.8660254037844387076, 1.000000000000000000, 0.9330127018922209636, 0.9330127018922194093 ) ) 
 REPRESENTATION_ITEM ( '' )  );
#18717 = CARTESIAN_POINT ( 'NONE',  ( 82.39999999999999147, -33.74062499938548854, -103.1828516163667899 ) ) ;
#18718 = EDGE_CURVE ( 'NONE', #15440, #2968, #15146, .T. ) ;
#18719 = CARTESIAN_POINT ( 'NONE',  ( 231.2217848218749339, -33.36562499938548143, -52.38713871227520968 ) ) ;
#18720 = CARTESIAN_POINT ( 'NONE',  ( -83.77821517812500929, -33.21562499938548285, 102.3871387122750889 ) ) ;
#18721 = ORIENTED_EDGE ( 'NONE', *, *, #14293, .T. ) ;
#18722 = CARTESIAN_POINT ( 'NONE',  ( 79.64356964375001269, -32.24062499938548854, 101.5914258081833879 ) ) ;
#18723 = CARTESIAN_POINT ( 'NONE',  ( 234.0999999999999375, -34.14374999877096428, -52.59807621135342970 ) ) ;
#18724 = CARTESIAN_POINT ( 'NONE',  ( -79.39999999999999147, -32.92500000000000426, 99.99999999999998579 ) ) ;
#18725 = FACE_OUTER_BOUND ( 'NONE', #16582, .T. ) ;
#18726 = CARTESIAN_POINT ( 'NONE',  ( -83.77821517812500929, -31.56562499938548427, 97.61286128772489690 ) ) ;
#18727 = DIRECTION ( 'NONE',  ( 1.000000000000000000, 0.000000000000000000, 0.000000000000000000 ) ) ;
#18728 = ORIENTED_EDGE ( 'NONE', *, *, #18695, .F. ) ;
#18729 = CARTESIAN_POINT ( 'NONE',  ( -82.39999999999999147, -33.48750000000000426, -96.53589838486223584 ) ) ;
#18730 = PRODUCT_DEFINITION_SHAPE ( 'NONE', 'NONE',  #15861 ) ;
#18731 = LINE ( 'NONE', #11093, #80 ) ;
#18732 = LINE ( 'NONE', #3868, #4528 ) ;
#18733 = CARTESIAN_POINT ( 'NONE',  ( -82.39999999999999147, -30.33356250001229171, 103.4641016151377499 ) ) ;
#18734 = CARTESIAN_POINT ( 'NONE',  ( 3.510273485745307731, 2.827716139362654424, -3.610536846335885564 ) ) ;
#18735 = EDGE_CURVE ( 'NONE', #8905, #4556, #7723, .T. ) ;
#18736 = CARTESIAN_POINT ( 'NONE',  ( -82.40000000000000568, -34.78124999877096712, 102.9999999999999858 ) ) ;
#18737 = CARTESIAN_POINT ( 'NONE',  ( -4.000000000000000000, -2.309401076758512694, -5.000000000000000000 ) ) ;
#18738 = CARTESIAN_POINT ( 'NONE',  ( -83.20384757729335945, -33.63615380933863008, -102.9999999999999716 ) ) ;
#18739 = CARTESIAN_POINT ( 'NONE',  ( 83.77821517812500929, -31.22812499938548569, 102.3871387122750889 ) ) ;
#18740 = CARTESIAN_POINT ( 'NONE',  ( 0.3126073911696462537, -4.041451884327388555, -1.676097590879904329E-16 ) ) ;
#18741 = CARTESIAN_POINT ( 'NONE',  ( -85.40000000000000568, -32.70000000000000284, -99.99999999999998579 ) ) ;
#18742 = CARTESIAN_POINT ( 'NONE',  ( 79.64356964375001269, -30.51562499938548711, -101.5914258081833879 ) ) ;
#18743 = DIRECTION ( 'NONE',  ( 0.000000000000000000, -1.000000000000000000, 0.000000000000000000 ) ) ;
#18744 = VERTEX_POINT ( 'NONE', #18281 ) ;
#18745 = CARTESIAN_POINT ( 'NONE',  ( 79.39999999999999147, -31.06874999877096855, 99.99999999999998579 ) ) ;
#18746 = SHAPE_DEFINITION_REPRESENTATION ( #16997, #14468 ) ;
#18747 = CARTESIAN_POINT ( 'NONE',  ( 235.3564303562499447, -34.56562499938547717, 101.5914258081833879 ) ) ;
#18748 = CARTESIAN_POINT ( 'NONE',  ( 235.3564303562499447, -33.17812499938548143, -50.00000000000011369 ) ) ;
#18749 = CARTESIAN_POINT ( 'NONE',  ( -85.15643035624999868, -32.80312499938548854, 101.5914258081833879 ) ) ;
#18750 = CARTESIAN_POINT ( 'NONE',  ( -84.59935209580211790, -35.00000000000002842, -98.20719995774828703 ) ) ;
#18751 = ORIENTED_EDGE ( 'NONE', *, *, #16270, .T. ) ;
#18752 = CARTESIAN_POINT ( 'NONE',  ( -81.02178482187500208, -31.34062499938548996, -97.61286128772489690 ) ) ;
#18753 = CARTESIAN_POINT ( 'NONE',  ( -82.40000000000000568, -30.95624999877097139, 96.99999999999998579 ) ) ;
#18754 = VERTEX_POINT ( 'NONE', #1764 ) ;
#18755 = CARTESIAN_POINT ( 'NONE',  ( 82.39999999999999147, -34.64062499938548711, 96.81714838363319586 ) ) ;
#18756 = CARTESIAN_POINT ( 'NONE',  ( -82.39999999999999147, -31.26562499938549067, -103.1828516163667899 ) ) ;
#18757 = CARTESIAN_POINT ( 'NONE',  ( 79.39999999999999147, -33.78750000000000142, 101.7320508075688821 ) ) ;
#18758 = CARTESIAN_POINT ( 'NONE',  ( -79.64057174634726266, -35.00000000000000000, 100.3964642588222063 ) ) ;
#18759 = CARTESIAN_POINT ( 'NONE',  ( -85.40000000000000568, -32.23124999877096997, 98.26794919243111792 ) ) ;
#18760 = CARTESIAN_POINT ( 'NONE',  ( -79.64356964374999848, -31.82812499938548356, 99.99999999999998579 ) ) ;
#18761 = CARTESIAN_POINT ( 'NONE',  ( -81.02178482187500208, -32.54062499938548569, -102.3871387122750889 ) ) ;
#18762 = CARTESIAN_POINT ( 'NONE',  ( 0.000000000000000000, 0.000000000000000000, -4.694516984716113228 ) ) ;
#18763 = CARTESIAN_POINT ( 'NONE',  ( 234.0999999999999375, -31.49999999999999289, 97.40192378864668399 ) ) ;
#18764 = ORIENTED_EDGE ( 'NONE', *, *, #2182, .T. ) ;
#18765 = CARTESIAN_POINT ( 'NONE',  ( 81.02178482187500208, -32.99062499938548854, -97.61286128772489690 ) ) ;
#18766 = CARTESIAN_POINT ( 'NONE',  ( 232.5999999999999375, -33.88124999877096144, 103.4641016151377499 ) ) ;
#18767 = CARTESIAN_POINT ( 'NONE',  ( 232.5999999999999375, -30.73124999877096286, -46.53589838486234953 ) ) ;
#18768 =( BOUNDED_CURVE ( )  B_SPLINE_CURVE ( 2, ( #1571, #6257, #12110, #13475, #12203, #15039, #8789, #19253, #14745 ),
 .UNSPECIFIED., .F., .F. ) 
 B_SPLINE_CURVE_WITH_KNOTS ( ( 3, 2, 2, 2, 3 ),
 ( 0.6875000000000000000, 0.6944444444444444198, 0.7083333333333333703, 0.7222222222222222099, 0.7291666666666666297 ),
 .UNSPECIFIED. ) 
 CURVE ( )  GEOMETRIC_REPRESENTATION_ITEM ( )  RATIONAL_B_SPLINE_CURVE ( ( 0.9330127018922194093, 0.9330127018922194093, 1.000000000000000000, 0.8660254037844387076, 1.000000000000000000, 0.8660254037844387076, 1.000000000000000000, 0.9330127018922198534, 0.9330127018922192983 ) ) 
 REPRESENTATION_ITEM ( '' )  );
#18769 = VERTEX_POINT ( 'NONE', #10461 ) ;
#18770 = CARTESIAN_POINT ( 'NONE',  ( -83.43214152715523824, -35.00000000000000000, 97.15572402832313514 ) ) ;
#18771 = CARTESIAN_POINT ( 'NONE',  ( -79.64356964374998427, -31.22812499938548569, 98.40857419181659793 ) ) ;
#18772 = FACE_OUTER_BOUND ( 'NONE', #4952, .T. ) ;
#18773 = EDGE_LOOP ( 'NONE', ( #10945, #2010, #7978, #8919 ) ) ;
#18774 = CARTESIAN_POINT ( 'NONE',  ( -83.90000000000000568, -34.06874999877096855, -102.5980762113533018 ) ) ;
#18775 = CARTESIAN_POINT ( 'NONE',  ( -79.39999999999999147, -33.76874999877097139, 99.99999999999998579 ) ) ;
#18776 = ORIENTED_EDGE ( 'NONE', *, *, #11887, .F. ) ;
#18777 = DIRECTION ( 'NONE',  ( 0.000000000000000000, -6.672013369141570147E-16, 1.000000000000000000 ) ) ;
#18778 = CARTESIAN_POINT ( 'NONE',  ( 85.40000000000000568, -33.14999999999999858, -99.99999999999998579 ) ) ;
#18779 = CARTESIAN_POINT ( 'NONE',  ( 84.29633955546289314, -32.00000000000002132, -102.0295751981968806 ) ) ;
#18780 = CARTESIAN_POINT ( 'NONE',  ( -83.77821517812500929, -32.57812499938548711, 97.61286128772489690 ) ) ;
#18781 = CARTESIAN_POINT ( 'NONE',  ( -80.90000000000000568, -30.75000000000000355, 102.5980762113533018 ) ) ;
#18782 = CARTESIAN_POINT ( 'NONE',  ( 235.3288510558096789, -34.99999999999999289, -50.77688434087658464 ) ) ;
#18783 = CARTESIAN_POINT ( 'NONE',  ( 231.4797793666090229, -31.99999999999997868, -52.57317574659983705 ) ) ;
#18784 = CARTESIAN_POINT ( 'NONE',  ( 82.39999999999999147, -34.64062499938548711, -103.1828516163667899 ) ) ;
#18785 = CARTESIAN_POINT ( 'NONE',  ( -82.40000000000001990, -33.26250000000000284, 97.00000000000000000 ) ) ;
#18786 = CARTESIAN_POINT ( 'NONE',  ( -85.15643035624999868, -34.60312499938548569, 101.5914258081833879 ) ) ;
#18787 = CARTESIAN_POINT ( 'NONE',  ( -82.39999999999999147, -31.23750000000000071, 102.9999999999999858 ) ) ;
#18788 = ORIENTED_EDGE ( 'NONE', *, *, #14718, .T. ) ;
#18789 = CARTESIAN_POINT ( 'NONE',  ( 234.0999999999999375, -34.79999999999999716, -47.40192378864679768 ) ) ;
#18790 = DIRECTION ( 'NONE',  ( 1.000000000000000000, 0.000000000000000000, 0.000000000000000000 ) ) ;
#18791 = AXIS2_PLACEMENT_3D ( 'NONE', #664, #852, #3476 ) ;
#18792 = AXIS2_PLACEMENT_3D ( 'NONE', #18581, #12805, #993 ) ;
#18793 =( BOUNDED_CURVE ( )  B_SPLINE_CURVE ( 2, ( #16086, #6915, #15800, #3970, #4263, #19114, #2500, #2405, #8369 ),
 .UNSPECIFIED., .F., .F. ) 
 B_SPLINE_CURVE_WITH_KNOTS ( ( 3, 2, 2, 2, 3 ),
 ( 0.3541666666666666297, 0.3611111111111111049, 0.3750000000000000000, 0.3888888888888888951, 0.3958333333333334259 ),
 .UNSPECIFIED. ) 
 CURVE ( )  GEOMETRIC_REPRESENTATION_ITEM ( )  RATIONAL_B_SPLINE_CURVE ( ( 0.9330127018922194093, 0.9330127018922190762, 1.000000000000000000, 0.8660254037844387076, 1.000000000000000000, 0.8660254037844387076, 1.000000000000000000, 0.9330127018922185211, 0.9330127018922192983 ) ) 
 REPRESENTATION_ITEM ( '' )  );
#18794 = CARTESIAN_POINT ( 'NONE',  ( -2.712762565639006418, 3.052587955997511759, -3.430618716626627318 ) ) ;
#18795 = CARTESIAN_POINT ( 'NONE',  ( 235.3564303562499447, -34.11562499938548143, 101.5914258081833879 ) ) ;
#18796 = CARTESIAN_POINT ( 'NONE',  ( -81.02178482187500208, -33.70312499938548711, 102.3871387122750889 ) ) ;
#18797 = CARTESIAN_POINT ( 'NONE',  ( 235.3564303562499447, -30.85312499938547859, -48.40857419181671162 ) ) ;
#18798 = EDGE_CURVE ( 'NONE', #7737, #4219, #18185, .T. ) ;
#18799 = VERTEX_POINT ( 'NONE', #11926 ) ;
#18800 = CARTESIAN_POINT ( 'NONE',  ( -82.65380294351676582, -34.99990492518305274, 97.01075526832239859 ) ) ;
#18801 = CARTESIAN_POINT ( 'NONE',  ( -79.64356964374999848, -34.86562499938548143, 99.99999999999998579 ) ) ;
#18802 = CARTESIAN_POINT ( 'NONE',  ( -83.04276107155152431, -35.00000000000000000, -102.9375709370400784 ) ) ;
#18803 = CARTESIAN_POINT ( 'NONE',  ( 83.77821517812500929, -32.46562499938548285, 102.3871387122750889 ) ) ;
#18804 = CARTESIAN_POINT ( 'NONE',  ( -4.140404888673278272, -2.228338276487456415, -3.686887068327035166 ) ) ;
#18805=STYLED_ITEM('',(#19343),#7516);
#18806 = CARTESIAN_POINT ( 'NONE',  ( -2.000000000000006661, 3.464101615137750834, 0.000000000000000000 ) ) ;
#18807 = ADVANCED_FACE ( 'NONE', ( #7625, #3423, #9373 ), #13680, .T. ) ;
#18808 = CARTESIAN_POINT ( 'NONE',  ( -85.15643035625001289, -34.71562499938548285, 101.5914258081833879 ) ) ;
#18809 = CARTESIAN_POINT ( 'NONE',  ( -83.77821517812500929, -33.02812499938548285, -102.3871387122750889 ) ) ;
#18810 = CARTESIAN_POINT ( 'NONE',  ( 83.77821517812500929, -31.56562499938548427, 102.3871387122750889 ) ) ;
#18811 = ADVANCED_FACE ( 'NONE', ( #16425 ), #289, .T. ) ;
#18812 = CARTESIAN_POINT ( 'NONE',  ( 82.39999999999999147, -34.64062499938548711, -103.1828516163667899 ) ) ;
#18813 = CARTESIAN_POINT ( 'NONE',  ( 235.3564303562499447, -32.65312499938547575, -48.40857419181671162 ) ) ;
#18814 = CARTESIAN_POINT ( 'NONE',  ( -79.64356964374999848, -33.96562499938548285, 99.99999999999998579 ) ) ;
#18815 = CARTESIAN_POINT ( 'NONE',  ( 83.77821517812500929, -31.11562499938548498, -97.61286128772489690 ) ) ;
#18816 = EDGE_CURVE ( 'NONE', #17634, #10576, #4632, .T. ) ;
#18817 = B_SPLINE_CURVE_WITH_KNOTS ( 'NONE', 3,
 ( #6114, #9129, #15092, #1708, #7663, #13618, #12163, #18613 ),
 .UNSPECIFIED., .F., .F.,
 ( 4, 2, 2, 4 ),
 ( 2.465131517075058656E-07, 0.001183067374689851080, 0.001774477805458923299, 0.002365888236227995517 ),
 .UNSPECIFIED. ) ;
#18818 = ORIENTED_EDGE ( 'NONE', *, *, #3851, .F. ) ;
#18819 = CARTESIAN_POINT ( 'NONE',  ( 82.39999999999999147, -34.19062499938548427, 96.81714838363319586 ) ) ;
#18820 = CARTESIAN_POINT ( 'NONE',  ( 0.5469614295415388128, -4.303013824935362663, -3.535263753543555598 ) ) ;
#18821 = CARTESIAN_POINT ( 'NONE',  ( -83.90000000000000568, -34.57500000000000284, 97.40192378864668399 ) ) ;
#18822 = AXIS2_PLACEMENT_3D ( 'NONE', #4676, #17868, #7692 ) ;
#18823 = CARTESIAN_POINT ( 'NONE',  ( -85.15643035624999868, -32.87812499938549138, 98.40857419181659793 ) ) ;
#18824 = CARTESIAN_POINT ( 'NONE',  ( -79.64356964374999848, -30.36562499938548498, 99.99999999999998579 ) ) ;
#18825 = CYLINDRICAL_SURFACE ( 'NONE', #18046, 3.000000000000002665 ) ;
#18826 = CARTESIAN_POINT ( 'NONE',  ( -85.12124608221316180, -31.99999999999999289, 99.52644304241999862 ) ) ;
#18827 = CARTESIAN_POINT ( 'NONE',  ( 235.3564303562499447, -32.57812499938548001, 98.40857419181659793 ) ) ;
#18828 = CARTESIAN_POINT ( 'NONE',  ( 83.95700771753406855, -35.00000000000000000, -97.42750194505821071 ) ) ;
#18829 = ADVANCED_FACE ( 'NONE', ( #9183 ), #12217, .F. ) ;
#18830 = CARTESIAN_POINT ( 'NONE',  ( -82.39999999999999147, -31.00856250001228887, 96.53589838486223584 ) ) ;
#18831 =( BOUNDED_CURVE ( )  B_SPLINE_CURVE ( 2, ( #10554, #8701, #4306, #5773, #1187, #11632, #16417, #13282, #2739 ),
 .UNSPECIFIED., .F., .F. ) 
 B_SPLINE_CURVE_WITH_KNOTS ( ( 3, 2, 2, 2, 3 ),
 ( 0.2291666666666666574, 0.2361111111111111049, 0.2500000000000000000, 0.2638888888888888951, 0.2708333333333333703 ),
 .UNSPECIFIED. ) 
 CURVE ( )  GEOMETRIC_REPRESENTATION_ITEM ( )  RATIONAL_B_SPLINE_CURVE ( ( 0.9330127018922194093, 0.9330127018922194093, 1.000000000000000000, 0.8660254037844387076, 1.000000000000000000, 0.8660254037844387076, 1.000000000000000000, 0.9330127018922190762, 0.9330127018922194093 ) ) 
 REPRESENTATION_ITEM ( '' )  );
#18832 = DIRECTION ( 'NONE',  ( 0.000000000000000000, 0.000000000000000000, -1.000000000000000000 ) ) ;
#18833 = CARTESIAN_POINT ( 'NONE',  ( 105.5000000000000142, 12.69999999999998508, 50.00000000000001421 ) ) ;
#18834 = DIRECTION ( 'NONE',  ( 0.000000000000000000, 0.000000000000000000, 1.000000000000000000 ) ) ;
#18835 = DIRECTION ( 'NONE',  ( 0.000000000000000000, 0.000000000000000000, 1.000000000000000000 ) ) ;
#18836 = CARTESIAN_POINT ( 'NONE',  ( 82.39999999999999147, -31.04062499938548569, 96.81714838363319586 ) ) ;
#18837 = CARTESIAN_POINT ( 'NONE',  ( 1.067261513540418550E-16, -0.3420925509381367302, 3.500000000000000000 ) ) ;
#18838 = CARTESIAN_POINT ( 'NONE',  ( 82.40000000000000568, -30.00000000000000355, -103.0000000000000000 ) ) ;
#18839 = CARTESIAN_POINT ( 'NONE',  ( 81.02178482187500208, -32.80312499938548854, -102.3871387122750889 ) ) ;
#18840 = ORIENTED_EDGE ( 'NONE', *, *, #5326, .F. ) ;
#18841 = CARTESIAN_POINT ( 'NONE',  ( 82.39999999999999147, -32.08124999877097139, 96.53589838486223584 ) ) ;
#18842 = CARTESIAN_POINT ( 'NONE',  ( 235.3564303562499447, -34.52812499938547575, 99.99999999999998579 ) ) ;
#18843 = EDGE_CURVE ( 'NONE', #11212, #14259, #17747, .T. ) ;
#18844 = CARTESIAN_POINT ( 'NONE',  ( 231.2217848218749339, -32.57812499938548001, -52.38713871227520968 ) ) ;
#18845 = CARTESIAN_POINT ( 'NONE',  ( -84.51154815724953551, -35.14114861271051637, 98.22820072003833047 ) ) ;
#18846 = CARTESIAN_POINT ( 'NONE',  ( 4.071447262713888016, -2.020725942163695166, -3.500000000000000000 ) ) ;
#18847 = EDGE_LOOP ( 'NONE', ( #10553, #1749, #9213, #9011 ) ) ;
#18848 = CARTESIAN_POINT ( 'NONE',  ( -81.02178482187500208, -31.79062499938548925, -97.61286128772489690 ) ) ;
#18849 = FACE_OUTER_BOUND ( 'NONE', #11718, .T. ) ;
#18850 = ORIENTED_EDGE ( 'NONE', *, *, #1016, .T. ) ;
#18851 = CARTESIAN_POINT ( 'NONE',  ( 79.64356964374999848, -32.72812499938548569, 99.99999999999998579 ) ) ;
#18852 = EDGE_CURVE ( 'NONE', #15758, #11084, #5263, .T. ) ;
#18853 = CARTESIAN_POINT ( 'NONE',  ( -81.02178482187500208, -31.45312499938549067, -97.61286128772489690 ) ) ;
#18854 = PRODUCT_RELATED_PRODUCT_CATEGORY ( 'part', '', ( #19045 ) ) ;
#18855 = CARTESIAN_POINT ( 'NONE',  ( 83.90000000000000568, -34.87500000000000000, 97.40192378864668399 ) ) ;
#18856 = DIRECTION ( 'NONE',  ( 0.000000000000000000, 0.000000000000000000, 1.000000000000000000 ) ) ;
#18857 = CARTESIAN_POINT ( 'NONE',  ( -85.40000000000000568, -35.30624999877096570, 101.7320508075688679 ) ) ;
#18858 = CARTESIAN_POINT ( 'NONE',  ( -81.02178482187500208, -30.40312499938548640, 97.61286128772489690 ) ) ;
#18859 = CARTESIAN_POINT ( 'NONE',  ( -85.15643035625001289, -33.32812499938548711, -101.5914258081833879 ) ) ;
#18860 = CARTESIAN_POINT ( 'NONE',  ( 233.5505106857032445, -35.00000000000000711, 102.5934467159355421 ) ) ;
#18861 = CARTESIAN_POINT ( 'NONE',  ( 85.40000000000000568, -30.84374999877096712, -99.99999999999998579 ) ) ;
#18862 = CARTESIAN_POINT ( 'NONE',  ( 232.5999999999999375, -31.46249999999999858, 96.53589838486223584 ) ) ;
#18863 = EDGE_LOOP ( 'NONE', ( #5293, #3530, #12492, #5006 ) ) ;
#18864 = CARTESIAN_POINT ( 'NONE',  ( 79.64356964374998427, -34.00312499938548427, -101.5914258081833879 ) ) ;
#18865 = CARTESIAN_POINT ( 'NONE',  ( 231.0999999999999375, -32.26874999877096428, 97.40192378864668399 ) ) ;
#18866 = FACE_OUTER_BOUND ( 'NONE', #381, .T. ) ;
#18867 = CARTESIAN_POINT ( 'NONE',  ( -84.13153929418699306, -35.00000000000000000, 97.51867099968119135 ) ) ;
#18868 = CARTESIAN_POINT ( 'NONE',  ( -83.77821517812500929, -30.51562499938548711, 102.3871387122750889 ) ) ;
#18869 = CARTESIAN_POINT ( 'NONE',  ( 79.39999999999997726, -32.01330983656912110, 100.5399455202950492 ) ) ;
#18870 = EDGE_LOOP ( 'NONE', ( #2763, #12487, #15831, #5581 ) ) ;
#18871 = CARTESIAN_POINT ( 'NONE',  ( 3.950241966888154987, -3.393956070637305089, 1.121495646999519202 ) ) ;
#18872 = AXIS2_PLACEMENT_3D ( 'NONE', #12345, #4835, #6785 ) ;
#18873 = CARTESIAN_POINT ( 'NONE',  ( 229.5999999999999375, -33.13124999877096144, 98.26794919243111792 ) ) ;
#18874 = ORIENTED_EDGE ( 'NONE', *, *, #3170, .T. ) ;
#18875 = SURFACE_STYLE_FILL_AREA ( #18686 ) ;
#18876 = CARTESIAN_POINT ( 'NONE',  ( 83.90000000000000568, -31.87500000000000000, -97.40192378864668399 ) ) ;
#18877 = LINE ( 'NONE', #20, #12665 ) ;
#18878 = CARTESIAN_POINT ( 'NONE',  ( -81.02178482187500208, -32.20312499938548711, 97.61286128772489690 ) ) ;
#18879 = CARTESIAN_POINT ( 'NONE',  ( -82.39999999999999147, -32.36250000000000426, 96.53589838486223584 ) ) ;
#18880 = CARTESIAN_POINT ( 'NONE',  ( 235.2646886264966497, -35.00000000000002132, -51.00543742925584212 ) ) ;
#18881 = CARTESIAN_POINT ( 'NONE',  ( 234.9223452063436639, -32.00000000000001421, -51.84871274668164176 ) ) ;
#18882 = CARTESIAN_POINT ( 'NONE',  ( 82.39999999999999147, -32.05312499938548854, 103.1828516163667899 ) ) ;
#18883 = DIRECTION ( 'NONE',  ( 0.000000000000000000, -1.000000000000000000, 0.000000000000000000 ) ) ;
#18884 = CARTESIAN_POINT ( 'NONE',  ( -83.77821517812500929, -35.01562499938548711, 102.3871387122750889 ) ) ;
#18885 =( BOUNDED_SURFACE ( )  B_SPLINE_SURFACE ( 1, 2, ( 
 ( #8432, #9907, #8338, #15958, #1024, #6976, #8527, #7166, #2564, #14477, #13024, #9104, #9198, #15067, #235, #16253, #7355, #340, #13312, #4626, #11847, #5992, #1598, #2862, #3052, #10579, #19286, #7453, #4425, #1688, #18204, #5901, #12236, #6191, #14975, #8911, #13411, #16636, #10667, #9015, #6287, #16545, #10384, #4823, #8819, #16346, #14775, #1403, #2956, #1779, #14872, #4724, #12039, #17815, #1501, #7640, #15161, #12141, #13594, #41, #6092, #17914, #4520, #11943, #13503, #18110, #10478, #142, #3144, #3240, #16443, #18013, #7545, #7741, #13699, #14081, #9692, #18691, #16835, #6476, #13884, #9297, #13791, #5205, #15460, #7837, #18491, #1976, #17121, #15262, #8129, #12520, #12429, #6771, #719, #9492, #2260, #2070, #15654, #11052, #18397, #8229, #435, #7933, #5017, #6675, #1877, #6380, #10958, #12616, #17021, #18298, #10763, #18589, #3631, #522, #3441, #12332, #11152, #4917, #3727, #9594, #16926, #3538, #14177, #8027, #2172, #10863, #812, #12719, #16728, #9392, #13986, #624, #15358 ),
 ( #3337, #6572, #5111, #15558, #1289, #15750, #6868, #16133, #3920, #14456, #4116, #10078, #8602, #2743, #11543, #17214, #8504, #909, #8704, #7147, #1192, #14552, #7237, #12910, #1088, #13192, #17313, #9887, #13098, #14654, #5687, #5308, #8318, #17411, #2356, #14366, #16036, #15849, #2542, #2458, #19068, #5598, #15940, #1003, #11250, #4024, #8414, #4211, #3819, #6958, #14272, #2637, #18878, #11636, #5500, #9788, #12815, #17598, #11447, #9985, #10170, #5405, #18780, #11348, #7046, #13004, #18975, #17505, #14848, #15045, #5776, #1576, #10362, #3029, #17795, #10558, #16519, #14951, #7524, #8989, #13480, #4405, #13387, #16326, #211, #120, #10455, #11828, #6167, #2935, #5971, #3122, #1757, #3219, #7332, #11728, #17696, #13285, #4696, #19260, #7620, #6069, #1385, #2840, #9079, #18088, #1668, #13572, #5878, #12015, #1473, #7430, #21, #16419, #12117, #4311, #17988, #4599, #10645, #9177, #16613, #8888, #15141, #7715, #19163, #10274, #16235, #11921, #17892, #4500, #8797, #14752, #8106, #18375, #10741 ) ),
 .UNSPECIFIED., .F., .F., .F. ) 
 B_SPLINE_SURFACE_WITH_KNOTS ( ( 2, 2 ),
 ( 3, 2, 2, 2, 2, 2, 2, 2, 2, 2, 2, 2, 2, 2, 2, 2, 2, 2, 2, 2, 2, 2, 2, 2, 2, 2, 2, 2, 2, 2, 2, 2, 2, 2, 2, 2, 2, 2, 2, 2, 2, 2, 2, 2, 2, 2, 2, 2, 2, 2, 2, 2, 2, 2, 2, 2, 2, 2, 2, 2, 2, 2, 2, 2, 2, 2, 2, 3 ),
 ( 0.000000000000000000, 1.000000000000000000 ),
 ( 0.000000000000000000, 0.01388888888888888812, 0.02777777777777777624, 0.04166666666666666435, 0.05555555555555555247, 0.06944444444444444753, 0.08333333333333332871, 0.09722222222222222376, 0.1111111111111111049, 0.1250000000000000000, 0.1388888888888888951, 0.1527777777777777901, 0.1666666666666666574, 0.1805555555555555525, 0.1944444444444444475, 0.2083333333333333426, 0.2222222222222222099, 0.2361111111111111049, 0.2500000000000000000, 0.2638888888888888951, 0.2777777777777777901, 0.2916666666666666852, 0.3055555555555555802, 0.3194444444444444198, 0.3333333333333333148, 0.3472222222222222099, 0.3611111111111111049, 0.3750000000000000000, 0.3888888888888888951, 0.4027777777777777901, 0.4166666666666666852, 0.4305555555555555802, 0.4444444444444444198, 0.4583333333333333148, 0.4722222222222222099, 0.4861111111111111049, 0.5000000000000000000, 0.5138888888888888395, 0.5277777777777777901, 0.5416666666666666297, 0.5555555555555555802, 0.5694444444444444198, 0.5833333333333333703, 0.5972222222222222099, 0.6111111111111111605, 0.6250000000000000000, 0.6388888888888888395, 0.6527777777777777901, 0.6666666666666666297, 0.6805555555555555802, 0.6944444444444444198, 0.7083333333333333703, 0.7222222222222222099, 0.7361111111111111605, 0.7500000000000000000, 0.7638888888888888395, 0.7777777777777777901, 0.7916666666666666297, 0.8055555555555555802, 0.8194444444444444198, 0.8333333333333333703, 0.8472222222222222099, 0.8611111111111111605, 0.8750000000000000000, 0.8888888888888888395, 0.9027777777777777901, 0.9166666666666666297, 0.9258785144422092550 ),
 .UNSPECIFIED. ) 
 GEOMETRIC_REPRESENTATION_ITEM ( )  RATIONAL_B_SPLINE_SURFACE ( (
 ( 1.000000000000000000, 0.8660254037844387076, 1.000000000000000000, 0.8660254037844387076, 1.000000000000000000, 0.8660254037844387076, 1.000000000000000000, 0.8660254037844387076, 1.000000000000000000, 0.8660254037844387076, 1.000000000000000000, 0.8660254037844387076, 1.000000000000000000, 0.8660254037844387076, 1.000000000000000000, 0.8660254037844387076, 1.000000000000000000, 0.8660254037844387076, 1.000000000000000000, 0.8660254037844387076, 1.000000000000000000, 0.8660254037844387076, 1.000000000000000000, 0.8660254037844387076, 1.000000000000000000, 0.8660254037844387076, 1.000000000000000000, 0.8660254037844387076, 1.000000000000000000, 0.8660254037844387076, 1.000000000000000000, 0.8660254037844387076, 1.000000000000000000, 0.8660254037844387076, 1.000000000000000000, 0.8660254037844387076, 1.000000000000000000, 0.8660254037844387076, 1.000000000000000000, 0.8660254037844387076, 1.000000000000000000, 0.8660254037844387076, 1.000000000000000000, 0.8660254037844387076, 1.000000000000000000, 0.8660254037844387076, 1.000000000000000000, 0.8660254037844387076, 1.000000000000000000, 0.8660254037844387076, 1.000000000000000000, 0.8660254037844387076, 1.000000000000000000, 0.8660254037844387076, 1.000000000000000000, 0.8660254037844387076, 1.000000000000000000, 0.8660254037844387076, 1.000000000000000000, 0.8660254037844387076, 1.000000000000000000, 0.8660254037844387076, 1.000000000000000000, 0.8660254037844387076, 1.000000000000000000, 0.8660254037844387076, 1.000000000000000000, 0.8660254037844387076, 1.000000000000000000, 0.8660254037844387076, 1.000000000000000000, 0.8660254037844387076, 1.000000000000000000, 0.8660254037844387076, 1.000000000000000000, 0.8660254037844387076, 1.000000000000000000, 0.8660254037844387076, 1.000000000000000000, 0.8660254037844387076, 1.000000000000000000, 0.8660254037844387076, 1.000000000000000000, 0.8660254037844387076, 1.000000000000000000, 0.8660254037844387076, 1.000000000000000000, 0.8660254037844387076, 1.000000000000000000, 0.8660254037844387076, 1.000000000000000000, 0.8660254037844387076, 1.000000000000000000, 0.8660254037844387076, 1.000000000000000000, 0.8660254037844387076, 1.000000000000000000, 0.8660254037844387076, 1.000000000000000000, 0.8660254037844387076, 1.000000000000000000, 0.8660254037844387076, 1.000000000000000000, 0.8660254037844387076, 1.000000000000000000, 0.8660254037844387076, 1.000000000000000000, 0.8660254037844387076, 1.000000000000000000, 0.8660254037844387076, 1.000000000000000000, 0.8660254037844387076, 1.000000000000000000, 0.8660254037844387076, 1.000000000000000000, 0.8660254037844387076, 1.000000000000000000, 0.8660254037844387076, 1.000000000000000000, 0.8660254037844387076, 1.000000000000000000, 0.8660254037844387076, 1.000000000000000000, 0.8660254037844387076, 1.000000000000000000, 0.8660254037844387076, 1.000000000000000000, 0.8660254037844387076, 1.000000000000000000, 0.8660254037844387076, 1.000000000000000000, 0.8660254037844387076, 1.000000000000000000, 0.9111409417988175496, 0.9401539645359766606),
 ( 1.000000000000000000, 0.8660254037844387076, 1.000000000000000000, 0.8660254037844387076, 1.000000000000000000, 0.8660254037844387076, 1.000000000000000000, 0.8660254037844387076, 1.000000000000000000, 0.8660254037844387076, 1.000000000000000000, 0.8660254037844387076, 1.000000000000000000, 0.8660254037844387076, 1.000000000000000000, 0.8660254037844387076, 1.000000000000000000, 0.8660254037844387076, 1.000000000000000000, 0.8660254037844387076, 1.000000000000000000, 0.8660254037844387076, 1.000000000000000000, 0.8660254037844387076, 1.000000000000000000, 0.8660254037844387076, 1.000000000000000000, 0.8660254037844387076, 1.000000000000000000, 0.8660254037844387076, 1.000000000000000000, 0.8660254037844387076, 1.000000000000000000, 0.8660254037844387076, 1.000000000000000000, 0.8660254037844387076, 1.000000000000000000, 0.8660254037844387076, 1.000000000000000000, 0.8660254037844387076, 1.000000000000000000, 0.8660254037844387076, 1.000000000000000000, 0.8660254037844387076, 1.000000000000000000, 0.8660254037844387076, 1.000000000000000000, 0.8660254037844387076, 1.000000000000000000, 0.8660254037844387076, 1.000000000000000000, 0.8660254037844387076, 1.000000000000000000, 0.8660254037844387076, 1.000000000000000000, 0.8660254037844387076, 1.000000000000000000, 0.8660254037844387076, 1.000000000000000000, 0.8660254037844387076, 1.000000000000000000, 0.8660254037844387076, 1.000000000000000000, 0.8660254037844387076, 1.000000000000000000, 0.8660254037844387076, 1.000000000000000000, 0.8660254037844387076, 1.000000000000000000, 0.8660254037844387076, 1.000000000000000000, 0.8660254037844387076, 1.000000000000000000, 0.8660254037844387076, 1.000000000000000000, 0.8660254037844387076, 1.000000000000000000, 0.8660254037844387076, 1.000000000000000000, 0.8660254037844387076, 1.000000000000000000, 0.8660254037844387076, 1.000000000000000000, 0.8660254037844387076, 1.000000000000000000, 0.8660254037844387076, 1.000000000000000000, 0.8660254037844387076, 1.000000000000000000, 0.8660254037844387076, 1.000000000000000000, 0.8660254037844387076, 1.000000000000000000, 0.8660254037844387076, 1.000000000000000000, 0.8660254037844387076, 1.000000000000000000, 0.8660254037844387076, 1.000000000000000000, 0.8660254037844387076, 1.000000000000000000, 0.8660254037844387076, 1.000000000000000000, 0.8660254037844387076, 1.000000000000000000, 0.8660254037844387076, 1.000000000000000000, 0.8660254037844387076, 1.000000000000000000, 0.8660254037844387076, 1.000000000000000000, 0.8660254037844387076, 1.000000000000000000, 0.8660254037844387076, 1.000000000000000000, 0.8660254037844387076, 1.000000000000000000, 0.8660254037844387076, 1.000000000000000000, 0.8660254037844387076, 1.000000000000000000, 0.8660254037844387076, 1.000000000000000000, 0.8660254037844387076, 1.000000000000000000, 0.8660254037844387076, 1.000000000000000000, 0.8660254037844387076, 1.000000000000000000, 0.8660254037844387076, 1.000000000000000000, 0.8660254037844387076, 1.000000000000000000, 0.9111409417988175496, 0.9401539645359766606) ) ) 
 REPRESENTATION_ITEM ( '' )  SURFACE ( )  );
#18886 = PLANE ( 'NONE',  #14897 ) ;
#18887 = ORIENTED_EDGE ( 'NONE', *, *, #2229, .F. ) ;
#18888 = CARTESIAN_POINT ( 'NONE',  ( 246.9999999999999716, -5.000000000000004441, 150.0000000000000000 ) ) ;
#18889 = FACE_OUTER_BOUND ( 'NONE', #17691, .T. ) ;
#18890 = AXIS2_PLACEMENT_3D ( 'NONE', #4087, #13160, #2998 ) ;
#18891 = PRODUCT ( 'MAS-172', 'MAS-172', '', ( #6833 ) ) ;
#18892 = CARTESIAN_POINT ( 'NONE',  ( -2.725741868435985094, 3.045094352034055429, -3.220599429844047012 ) ) ;
#18893 = FACE_OUTER_BOUND ( 'NONE', #2230, .T. ) ;
#18894 = CARTESIAN_POINT ( 'NONE',  ( -79.64356964375001269, -32.69062499938548427, 98.40857419181659793 ) ) ;
#18895 = CARTESIAN_POINT ( 'NONE',  ( 230.4884518427504076, -35.25364861271050643, -51.77179927996177611 ) ) ;
#18896 = ORIENTED_EDGE ( 'NONE', *, *, #10788, .T. ) ;
#18897 = CARTESIAN_POINT ( 'NONE',  ( -82.39999999999999147, -34.30312499938548143, 96.81714838363319586 ) ) ;
#18898 = LINE ( 'NONE', #12836, #14729 ) ;
#18899 = CARTESIAN_POINT ( 'NONE',  ( 85.15643035624999868, -34.15312499938548285, 98.40857419181659793 ) ) ;
#18900 = CARTESIAN_POINT ( 'NONE',  ( 105.1999999999999744, -4.999999999999976907, 150.0000000000000000 ) ) ;
#18901 = CARTESIAN_POINT ( 'NONE',  ( 110.0000000000000000, 5.199999999999953104, 41.33974596215564645 ) ) ;
#18902 = CARTESIAN_POINT ( 'NONE',  ( -79.64356964374998427, -34.94062499938548427, 98.40857419181659793 ) ) ;
#18903 = CARTESIAN_POINT ( 'NONE',  ( -85.15643035625001289, -33.89062499938548711, -101.5914258081833879 ) ) ;
#18904 = CARTESIAN_POINT ( 'NONE',  ( 81.02178482187500208, -32.99062499938548854, 102.3871387122750889 ) ) ;
#18905 = EDGE_CURVE ( 'NONE', #16451, #16118, #18931, .T. ) ;
#18906 = EDGE_CURVE ( 'NONE', #13209, #3413, #6212, .T. ) ;
#18907 = CARTESIAN_POINT ( 'NONE',  ( 79.64356964375001269, -33.66562499938549280, -101.5914258081833879 ) ) ;
#18908 = CARTESIAN_POINT ( 'NONE',  ( 235.3564303562499447, -33.92812499938548143, -51.59142580818350865 ) ) ;
#18909 = CARTESIAN_POINT ( 'NONE',  ( -83.77821517812500929, -34.11562499938548854, 102.3871387122750889 ) ) ;
#18910 = CARTESIAN_POINT ( 'NONE',  ( 82.39999999999999147, -31.82812499938548356, -103.1828516163667899 ) ) ;
#18911 = ORIENTED_EDGE ( 'NONE', *, *, #2906, .T. ) ;
#18912 = CARTESIAN_POINT ( 'NONE',  ( 85.15643035624999868, -34.34062499938548285, 101.5914258081833879 ) ) ;
#18913 = CARTESIAN_POINT ( 'NONE',  ( 232.5999999999999375, -34.33124999877097139, -47.00000000000011369 ) ) ;
#18914 = CARTESIAN_POINT ( 'NONE',  ( -83.90000000000000568, -33.97500000000000853, 102.5980762113533018 ) ) ;
#18915 = VECTOR ( 'NONE', #1667, 1000.000000000000000 ) ;
#18916 = CARTESIAN_POINT ( 'NONE',  ( -83.77821517812500929, -32.76562499938548711, 102.3871387122750889 ) ) ;
#18917 = CARTESIAN_POINT ( 'NONE',  ( -83.77821517812500929, -31.41562499938548569, 102.3871387122750889 ) ) ;
#18919 = EDGE_CURVE ( 'NONE', #5195, #10996, #8557, .T. ) ;
#18918 = CARTESIAN_POINT ( 'NONE',  ( 83.90000000000000568, -34.87500000000000000, 97.40192378864668399 ) ) ;
#18920 = ADVANCED_FACE ( 'NONE', ( #14509 ), #11209, .T. ) ;
#18921 = CARTESIAN_POINT ( 'NONE',  ( 231.2217848218749339, -32.01562499938548001, 97.61286128772489690 ) ) ;
#18922 = CARTESIAN_POINT ( 'NONE',  ( 232.5999999999999375, -29.99999999999999645, 103.0000000000000000 ) ) ;
#18923 = CARTESIAN_POINT ( 'NONE',  ( 82.40000000000000568, -33.71249999999998437, -96.99999999999998579 ) ) ;
#18924 = EDGE_CURVE ( 'NONE', #1776, #18769, #17174, .T. ) ;
#18925 = CARTESIAN_POINT ( 'NONE',  ( -85.40000000000000568, -34.85624999877096997, 101.7320508075688821 ) ) ;
#18926 = CARTESIAN_POINT ( 'NONE',  ( -80.90000000000000568, -33.24374999877097281, -102.5980762113533018 ) ) ;
#18927 = CARTESIAN_POINT ( 'NONE',  ( -85.40000000000000568, -33.56250000000000000, 101.7320508075688821 ) ) ;
#18928 = DIRECTION ( 'NONE',  ( -0.000000000000000000, 0.000000000000000000, -1.000000000000000000 ) ) ;
#18929 = VECTOR ( 'NONE', #7302, 1000.000000000000000 ) ;
#18930 = LINE ( 'NONE', #13057, #6475 ) ;
#18931 = LINE ( 'NONE', #18838, #4648 ) ;
#18932 = CARTESIAN_POINT ( 'NONE',  ( 85.15643035624999868, -33.89062499938548711, -98.40857419181659793 ) ) ;
#18933 = CARTESIAN_POINT ( 'NONE',  ( 4.158413352280808439, 2.044871626972822209, 3.541821552872961298 ) ) ;
#18934 = ORIENTED_EDGE ( 'NONE', *, *, #6579, .T. ) ;
#18935 = CARTESIAN_POINT ( 'NONE',  ( 80.90000000000000568, -32.49374999877097281, 97.40192378864668399 ) ) ;
#18936 = ITEM_DEFINED_TRANSFORMATION ( 'NONE', 'NONE', #12676,  #10540 ) ;
#18937 = CARTESIAN_POINT ( 'NONE',  ( -82.40000000000000568, -31.63124999877096855, 102.9999999999999858 ) ) ;
#18938 = CARTESIAN_POINT ( 'NONE',  ( 232.5999999999999375, -33.51562499938548001, -53.18285161636690361 ) ) ;
#18939 = FACE_OUTER_BOUND ( 'NONE', #1867, .T. ) ;
#18940 = DIRECTION ( 'NONE',  ( 0.000000000000000000, 0.000000000000000000, -1.000000000000000000 ) ) ;
#18941 = VERTEX_POINT ( 'NONE', #13058 ) ;
#18942 = CARTESIAN_POINT ( 'NONE',  ( -82.39999999999999147, -33.40312499938548285, -103.1828516163667899 ) ) ;
#18943 = DIRECTION ( 'NONE',  ( 1.000000000000000000, 0.000000000000000000, 0.000000000000000000 ) ) ;
#18944 = VERTEX_POINT ( 'NONE', #12667 ) ;
#18945 =( REPRESENTATION_RELATIONSHIP ('NONE','NONE', #14468, #9634 ) REPRESENTATION_RELATIONSHIP_WITH_TRANSFORMATION ( #15903 )SHAPE_REPRESENTATION_RELATIONSHIP( ) );
#18946 = CARTESIAN_POINT ( 'NONE',  ( 85.15643035625001289, -33.89062499938548711, 101.5914258081833879 ) ) ;
#18947 = CARTESIAN_POINT ( 'NONE',  ( -83.77821517812500929, -31.22812499938548569, -102.3871387122750889 ) ) ;
#18948 = CARTESIAN_POINT ( 'NONE',  ( 80.90000000000000568, -34.64999999999999858, 102.5980762113533018 ) ) ;
#18949 = CARTESIAN_POINT ( 'NONE',  ( 81.59615242270662350, -34.76115380933863719, -103.0000000000000000 ) ) ;
#18950 = CARTESIAN_POINT ( 'NONE',  ( -85.40000000000000568, -30.39768749875867826, 99.99999999999998579 ) ) ;
#18951 = AXIS2_PLACEMENT_3D ( 'NONE', #6662, #11137, #10755 ) ;
#18952 = CARTESIAN_POINT ( 'NONE',  ( -79.64356964375001269, -30.51562499938548711, 101.5914258081833879 ) ) ;
#18953 = CARTESIAN_POINT ( 'NONE',  ( -85.15643035625001289, -32.87812499938548427, -101.5914258081833879 ) ) ;
#18954 = CARTESIAN_POINT ( 'NONE',  ( 233.0319854768594041, -35.00000000000000000, 102.7281823352557097 ) ) ;
#18955 = CARTESIAN_POINT ( 'NONE',  ( 79.39999999999999147, -32.41874999877096997, -99.99999999999998579 ) ) ;
#18956 = AXIS2_PLACEMENT_3D ( 'NONE', #12073, #15101, #6027 ) ;
#18957 = CARTESIAN_POINT ( 'NONE',  ( 235.5999999999999943, -32.06249999999999289, 101.7320508075688537 ) ) ;
#18958 = VERTEX_POINT ( 'NONE', #6918 ) ;
#18959 = DIRECTION ( 'NONE',  ( -0.000000000000000000, -0.000000000000000000, 1.000000000000000000 ) ) ;
#18960 = DIRECTION ( 'NONE',  ( 0.000000000000000000, 0.000000000000000000, 1.000000000000000000 ) ) ;
#18961 = EDGE_CURVE ( 'NONE', #3695, #11655, #5648, .T. ) ;
#18962 = CARTESIAN_POINT ( 'NONE',  ( 229.5999999999999375, -33.09374999877096002, 99.99999999999998579 ) ) ;
#18963 = CARTESIAN_POINT ( 'NONE',  ( 234.0999999999999375, -30.99374999877096215, -52.59807621135342970 ) ) ;
#18964 = CARTESIAN_POINT ( 'NONE',  ( 231.0999999999999375, -34.57499999999999574, 97.40192378864668399 ) ) ;
#18965 = CARTESIAN_POINT ( 'NONE',  ( -79.64356964374999848, -31.71562499938548285, 99.99999999999998579 ) ) ;
#18966 = AXIS2_PLACEMENT_3D ( 'NONE', #10875, #12346, #732 ) ;
#18967 = ORIENTED_EDGE ( 'NONE', *, *, #7239, .T. ) ;
#18968 = EDGE_LOOP ( 'NONE', ( #15036, #10263, #2897, #2675 ) ) ;
#18969 = CARTESIAN_POINT ( 'NONE',  ( 4.175326769692873974, -4.121399112977854884, -1.039526559595160114E-14 ) ) ;
#18970 = VERTEX_POINT ( 'NONE', #505 ) ;
#18971 = CARTESIAN_POINT ( 'NONE',  ( 85.40000000000000568, -31.76249999999999929, -101.7320508075688679 ) ) ;
#18972 = CARTESIAN_POINT ( 'NONE',  ( 81.01744233620649993, -31.99999999999999289, -102.5835086888312162 ) ) ;
#18973 = AXIS2_PLACEMENT_3D ( 'NONE', #17995, #9184, #9087 ) ;
#18974 = AXIS2_PLACEMENT_3D ( 'NONE', #14612, #11877, #13531 ) ;
#18975 = CARTESIAN_POINT ( 'NONE',  ( -79.64356964374999848, -32.72812499938548569, 99.99999999999998579 ) ) ;
#18976 = CARTESIAN_POINT ( 'NONE',  ( -79.39999999999999147, -31.57499999999999929, 99.99999999999998579 ) ) ;
#18977 = CARTESIAN_POINT ( 'NONE',  ( 233.5509609210265296, -31.99999999999997868, -52.74042984513003063 ) ) ;
#18978 = DIRECTION ( 'NONE',  ( 1.000000000000000000, -0.000000000000000000, -0.000000000000000000 ) ) ;
#18979 = VECTOR ( 'NONE', #18552, 1000.000000000000000 ) ;
#18980 = CARTESIAN_POINT ( 'NONE',  ( 81.05805657947855991, -35.00000000000000711, 102.6149389257479640 ) ) ;
#18981 = CARTESIAN_POINT ( 'NONE',  ( 84.25709831968876529, -34.99999999999999289, 97.88253972981353002 ) ) ;
#18982 = CARTESIAN_POINT ( 'NONE',  ( 85.15643035624999868, -35.05312499938548143, -101.5914258081833879 ) ) ;
#18983 = ORIENTED_EDGE ( 'NONE', *, *, #4026, .T. ) ;
#18984 =( NAMED_UNIT ( * ) SI_UNIT ( $, .STERADIAN. ) SOLID_ANGLE_UNIT ( ) );
#18985 = CARTESIAN_POINT ( 'NONE',  ( -81.02178482187500208, -31.19062499938548427, -102.3871387122750889 ) ) ;
#18986 = CARTESIAN_POINT ( 'NONE',  ( 232.5880334581522391, -34.99999999999999289, 97.00083539721710224 ) ) ;
#18987 = AXIS2_PLACEMENT_3D ( 'NONE', #1008, #6963, #5021 ) ;
#18988 = VECTOR ( 'NONE', #10912, 1000.000000000000000 ) ;
#18989 = CARTESIAN_POINT ( 'NONE',  ( -81.59615242270662350, -33.41115380933863577, 102.9999999999999858 ) ) ;
#18990 = CARTESIAN_POINT ( 'NONE',  ( 235.3564303562499447, -34.56562499938547717, 101.5914258081833879 ) ) ;
#18991 = CARTESIAN_POINT ( 'NONE',  ( -81.02178482187500208, -34.15312499938548285, 102.3871387122750889 ) ) ;
#18992 = DIRECTION ( 'NONE',  ( 0.7660487055105749121, 0.000000000000000000, 0.6427825299318367103 ) ) ;
#18993 = CARTESIAN_POINT ( 'NONE',  ( 229.8435696437499871, -34.79062499938547859, -51.59142580818350865 ) ) ;
#18994 = EDGE_LOOP ( 'NONE', ( #1851, #18480, #6123, #11511 ) ) ;
#18995 = CARTESIAN_POINT ( 'NONE',  ( -85.15643035625001289, -34.64062499938548711, 99.99999999999998579 ) ) ;
#18996 = CARTESIAN_POINT ( 'NONE',  ( 83.25523545990762386, -35.19352049914630953, 103.2690260512239604 ) ) ;
#18997 = CARTESIAN_POINT ( 'NONE',  ( -82.40000000000000568, -33.71249999999998437, 96.99999999999998579 ) ) ;
#18998 = AXIS2_PLACEMENT_3D ( 'NONE', #13392, #10652, #10748 ) ;
#18999 = CARTESIAN_POINT ( 'NONE',  ( 235.3564303562499447, -32.65312499938547575, 101.5914258081833879 ) ) ;
#19000 = CYLINDRICAL_SURFACE ( 'NONE', #12963, 3.000000000000002665 ) ;
#19001 = CARTESIAN_POINT ( 'NONE',  ( -81.02178482187500208, -33.55312499938548854, 97.61286128772489690 ) ) ;
#19002 = CARTESIAN_POINT ( 'NONE',  ( -81.02178482187500208, -33.70312499938548711, -97.61286128772489690 ) ) ;
#19003 = DIRECTION ( 'NONE',  ( -1.000000000000000000, -0.000000000000000000, -0.000000000000000000 ) ) ;
#19004 = CARTESIAN_POINT ( 'NONE',  ( 81.02178482187500208, -33.10312499938548569, -97.61286128772489690 ) ) ;
#19005 = CARTESIAN_POINT ( 'NONE',  ( 231.2217848218749339, -34.26562499938548001, -52.38713871227520968 ) ) ;
#19006 = CARTESIAN_POINT ( 'NONE',  ( -85.15643035625001289, -34.15312499938548285, 101.5914258081833879 ) ) ;
#19007 = CARTESIAN_POINT ( 'NONE',  ( 79.64356964375001269, -30.40312499938548285, -101.5914258081833879 ) ) ;
#19008 = EDGE_LOOP ( 'NONE', ( #8873, #686, #3716, #18370 ) ) ;
#19009 = CARTESIAN_POINT ( 'NONE',  ( 81.02178482187500208, -34.45312499938548711, 102.3871387122750889 ) ) ;
#19010 = CARTESIAN_POINT ( 'NONE',  ( 3.455068668934414777, -2.624017327439094327, -3.316620875263732504 ) ) ;
#19011 = CARTESIAN_POINT ( 'NONE',  ( -80.90000000000000568, -33.30000000000000426, 97.40192378864668399 ) ) ;
#19012 = CARTESIAN_POINT ( 'NONE',  ( -79.64356964374999848, -34.41562499938548569, 99.99999999999998579 ) ) ;
#19013 = CARTESIAN_POINT ( 'NONE',  ( -83.77821517812500929, -30.51562499938548711, 102.3871387122750889 ) ) ;
#19014 = VERTEX_POINT ( 'NONE', #5460 ) ;
#19015 = DIRECTION ( 'NONE',  ( 0.000000000000000000, 0.000000000000000000, -1.000000000000000000 ) ) ;
#19016 = CARTESIAN_POINT ( 'NONE',  ( 232.5999999999999943, -33.40312499938547575, 96.81714838363319586 ) ) ;
#19017 = DIRECTION ( 'NONE',  ( 1.000000000000000000, -1.387778780781445478E-15, 0.000000000000000000 ) ) ;
#19018 = CARTESIAN_POINT ( 'NONE',  ( -83.90000000000000568, -34.42500000000000426, 102.5980762113533018 ) ) ;
#19019 = DIRECTION ( 'NONE',  ( -0.000000000000000000, 0.000000000000000000, -1.000000000000000000 ) ) ;
#19020 = CARTESIAN_POINT ( 'NONE',  ( -79.39999999999999147, -33.35624999877096997, -98.26794919243113213 ) ) ;
#19021 = CARTESIAN_POINT ( 'NONE',  ( 84.93334430221547393, -32.00000000000000000, 98.89901723338974193 ) ) ;
#19022 = CARTESIAN_POINT ( 'NONE',  ( 79.64356964375001269, -32.24062499938548854, 101.5914258081833879 ) ) ;
#19023 = DIRECTION ( 'NONE',  ( 0.000000000000000000, 0.000000000000000000, -1.000000000000000000 ) ) ;
#19024 = DIRECTION ( 'NONE',  ( -0.000000000000000000, -1.000000000000000000, -0.000000000000000000 ) ) ;
#19025 = CARTESIAN_POINT ( 'NONE',  ( 85.15643035625001289, -33.85312499938549280, -99.99999999999998579 ) ) ;
#19026 = CARTESIAN_POINT ( 'NONE',  ( 79.39999999999999147, -32.86874999877097281, 99.99999999999998579 ) ) ;
#19027 = ORIENTED_EDGE ( 'NONE', *, *, #2123, .T. ) ;
#19028 = CARTESIAN_POINT ( 'NONE',  ( 82.39999999999999147, -32.75624999877096855, 103.4641016151377499 ) ) ;
#19029 = CARTESIAN_POINT ( 'NONE',  ( 233.9782151781249411, -34.60312499938548569, 102.3871387122750889 ) ) ;
#19030 = CARTESIAN_POINT ( 'NONE',  ( 235.3564303562499447, -34.56562499938547717, -48.40857419181671162 ) ) ;
#19031 = CARTESIAN_POINT ( 'NONE',  ( 82.40000000000000568, -34.38749999999999574, 96.99999999999998579 ) ) ;
#19032 = CARTESIAN_POINT ( 'NONE',  ( 3.951447005078451813, -2.357513599190978137, -2.916666666666667407 ) ) ;
#19033 = VERTEX_POINT ( 'NONE', #9744 ) ;
#19034 = CARTESIAN_POINT ( 'NONE',  ( -82.39999999999999147, -34.30312499938548143, -103.1828516163667899 ) ) ;
#19035 = CARTESIAN_POINT ( 'NONE',  ( 85.40000000000000568, -33.14999999999999858, 99.99999999999998579 ) ) ;
#19036 = EDGE_CURVE ( 'NONE', #15781, #13743, #16366, .T. ) ;
#19037 = ORIENTED_EDGE ( 'NONE', *, *, #11980, .T. ) ;
#19038 = CARTESIAN_POINT ( 'NONE',  ( 82.39999999999999147, -34.86562499938548854, 103.1828516163667899 ) ) ;
#19039 = CARTESIAN_POINT ( 'NONE',  ( -79.39999999999999147, -35.08124999877097139, -101.7320508075688821 ) ) ;
#19040 = CARTESIAN_POINT ( 'NONE',  ( -83.90000000000000568, -32.11874999877097281, -97.40192378864668399 ) ) ;
#19041 = LINE ( 'NONE', #1068, #15692 ) ;
#19042 = CARTESIAN_POINT ( 'NONE',  ( -83.90000000000000568, -34.06874999877096855, 97.40192378864668399 ) ) ;
#19043 = CARTESIAN_POINT ( 'NONE',  ( -85.15643035624999868, -31.64062499938548356, 98.40857419181659793 ) ) ;
#19044 = CARTESIAN_POINT ( 'NONE',  ( -79.64356964374998427, -33.02812499938548285, -101.5914258081833879 ) ) ;
#19045 = PRODUCT ( 'grip', 'grip', '', ( #13945 ) ) ;
#19046 = CARTESIAN_POINT ( 'NONE',  ( 235.0940413310670465, -34.99999999999999289, 101.1871036926526557 ) ) ;
#19047 = EDGE_CURVE ( 'NONE', #15577, #14, #17364, .T. ) ;
#19048 = CARTESIAN_POINT ( 'NONE',  ( 80.90000000000000568, -32.49374999877097281, -102.5980762113533018 ) ) ;
#19049 = CARTESIAN_POINT ( 'NONE',  ( 229.5999999999999375, -30.93749999999999289, 98.26794919243111792 ) ) ;
#19050 = EDGE_CURVE ( 'NONE', #13807, #13667, #13060, .T. ) ;
#19051 = ORIENTED_EDGE ( 'NONE', *, *, #7495, .T. ) ;
#19052 = CARTESIAN_POINT ( 'NONE',  ( 81.02178482187500208, -34.34062499938548285, -97.61286128772489690 ) ) ;
#19053 = FILL_AREA_STYLE ('',( #4102 ) ) ;
#19054 = CARTESIAN_POINT ( 'NONE',  ( 231.0999999999999375, -31.81874999877096144, 97.40192378864668399 ) ) ;
#19055 = CARTESIAN_POINT ( 'NONE',  ( 232.5999999999999375, -31.18124999877096215, -46.53589838486234953 ) ) ;
#19056 = EDGE_CURVE ( 'NONE', #6865, #11363, #7141, .T. ) ;
#19057 = CARTESIAN_POINT ( 'NONE',  ( -80.90000000000000568, -35.04374999877096997, 97.40192378864668399 ) ) ;
#19058 = CARTESIAN_POINT ( 'NONE',  ( -85.15643035625001289, -31.90312499938548285, 101.5914258081833879 ) ) ;
#19059 = ORIENTED_EDGE ( 'NONE', *, *, #2950, .F. ) ;
#19060 = VERTEX_POINT ( 'NONE', #8940 ) ;
#19061 = CARTESIAN_POINT ( 'NONE',  ( 81.59615242270662350, -34.36740381056766580, -102.9999999999999858 ) ) ;
#19062 = CARTESIAN_POINT ( 'NONE',  ( 4.211140560182196957, -2.431303136016555122, -3.745885042887436622 ) ) ;
#19063 = ORIENTED_EDGE ( 'NONE', *, *, #3264, .F. ) ;
#19064 = B_SPLINE_CURVE_WITH_KNOTS ( 'NONE', 3,
 ( #8606, #10277, #14659, #17700, #17603, #18980, #4409, #2641, #8509, #4216, #8707, #2547, #4316, #7436, #16239, #1195, #8802, #17418 ),
 .UNSPECIFIED., .F., .F.,
 ( 4, 2, 2, 2, 2, 2, 2, 2, 4 ),
 ( 0.000000000000000000, 0.0007106627595359126057, 0.001421325519071825211, 0.002131988278607738034, 0.002842651038143650423, 0.003553313797679562812, 0.004263976557215476068, 0.004974639316751388457, 0.005685302076287300846 ),
 .UNSPECIFIED. ) ;
#19065 = CARTESIAN_POINT ( 'NONE',  ( 4.000000000000000000, -2.309401076758514915, -3.433295621305383349 ) ) ;
#19066 = CARTESIAN_POINT ( 'NONE',  ( 80.90000000000000568, -31.65000000000000568, -102.5980762113533018 ) ) ;
#19067 = CARTESIAN_POINT ( 'NONE',  ( 94.79999999999995453, -35.00000000000000000, 150.0000000000000000 ) ) ;
#19068 = CARTESIAN_POINT ( 'NONE',  ( -81.02178482187500208, -31.75312499938548427, 97.61286128772489690 ) ) ;
#19069 = CARTESIAN_POINT ( 'NONE',  ( -79.39999999999999147, -32.51250000000000284, 101.7320508075688537 ) ) ;
#19070 = EDGE_CURVE ( 'NONE', #17663, #11212, #19106, .T. ) ;
#19071 = LINE ( 'NONE', #13006, #14600 ) ;
#19072 = CARTESIAN_POINT ( 'NONE',  ( -84.69814171518287083, -35.32864829504264748, 98.07164716482272127 ) ) ;
#19073 = DIRECTION ( 'NONE',  ( -1.000000000000000000, -0.000000000000000000, 0.000000000000000000 ) ) ;
#19074 = CARTESIAN_POINT ( 'NONE',  ( -85.40000000000000568, -34.53750000000000142, -101.7320508075688821 ) ) ;
#19075 = ORIENTED_EDGE ( 'NONE', *, *, #892, .T. ) ;
#19076 = CARTESIAN_POINT ( 'NONE',  ( -81.02178482187500208, -31.64062499938548356, -102.3871387122750889 ) ) ;
#19077 = CARTESIAN_POINT ( 'NONE',  ( 235.2218879900010791, -34.99999999999999289, 100.8506536761482124 ) ) ;
#19078 = FACE_OUTER_BOUND ( 'NONE', #661, .T. ) ;
#19079 = CARTESIAN_POINT ( 'NONE',  ( 235.3564303562499447, -34.52812499938547575, 99.99999999999998579 ) ) ;
#19080 = CARTESIAN_POINT ( 'NONE',  ( -83.77821517812500929, -31.11562499938548498, 97.61286128772489690 ) ) ;
#19081 = CARTESIAN_POINT ( 'NONE',  ( 82.39999999999999147, -32.58749999999999858, 96.99999999999998579 ) ) ;
#19082 = ADVANCED_FACE ( 'NONE', ( #17941 ), #19215, .T. ) ;
#19083 = CARTESIAN_POINT ( 'NONE',  ( 235.3564303562499447, -33.10312499938547859, -48.40857419181671162 ) ) ;
#19084 = ORIENTED_EDGE ( 'NONE', *, *, #2361, .T. ) ;
#19085 = EDGE_LOOP ( 'NONE', ( #19281, #12178, #3811, #427 ) ) ;
#19086 = CARTESIAN_POINT ( 'NONE',  ( -85.15643035624999868, -34.22812499938547859, 98.40857419181659793 ) ) ;
#19087 = CARTESIAN_POINT ( 'NONE',  ( -82.40000000000000568, -30.00000000000000355, 96.99999999999998579 ) ) ;
#19088 = CARTESIAN_POINT ( 'NONE',  ( 79.64356964375001269, -34.90312499938548285, 98.40857419181659793 ) ) ;
#19089 = LINE ( 'NONE', #1211, #4001 ) ;
#19090 = CARTESIAN_POINT ( 'NONE',  ( 231.2217848218749339, -31.86562499938547788, 102.3871387122750889 ) ) ;
#19091 = CARTESIAN_POINT ( 'NONE',  ( 229.8435696437499587, -32.87812499938547717, -51.59142580818350154 ) ) ;
#19092 = CARTESIAN_POINT ( 'NONE',  ( -79.39999999999999147, -33.86250000000000426, 101.7320508075688537 ) ) ;
#19093 = CARTESIAN_POINT ( 'NONE',  ( 85.40000000000000568, -33.05624999877097281, -101.7320508075688821 ) ) ;
#19094 = CARTESIAN_POINT ( 'NONE',  ( 79.64356964375001269, -31.67812499938548143, -98.40857419181659793 ) ) ;
#19095 = CARTESIAN_POINT ( 'NONE',  ( 229.5999999999999375, -31.38749999999999218, -51.73205080756898866 ) ) ;
#19096 = CARTESIAN_POINT ( 'NONE',  ( -83.77821517812500929, -32.76562499938548711, 102.3871387122750889 ) ) ;
#19097 = CARTESIAN_POINT ( 'NONE',  ( 83.77821517812500929, -30.66562499938548569, -97.61286128772489690 ) ) ;
#19098 = EDGE_LOOP ( 'NONE', ( #10306, #9353, #6318 ) ) ;
#19099 = CARTESIAN_POINT ( 'NONE',  ( 232.5999999999999375, -29.99999999999999645, -50.00000000000011369 ) ) ;
#19100 = DIRECTION ( 'NONE',  ( -0.000000000000000000, -0.000000000000000000, 1.000000000000000000 ) ) ;
#19101 = CARTESIAN_POINT ( 'NONE',  ( 232.5999999999999375, -30.81562499938547717, -53.18285161636690361 ) ) ;
#19102 = CARTESIAN_POINT ( 'NONE',  ( -81.02178482187500208, -32.69062499938548427, 102.3871387122750889 ) ) ;
#19103 = VERTEX_POINT ( 'NONE', #13143 ) ;
#19104 = CARTESIAN_POINT ( 'NONE',  ( -4.101948962586059899, -2.368261337751176754, -3.681124513963741851 ) ) ;
#19105 = VECTOR ( 'NONE', #3310, 1000.000000000000000 ) ;
#19106 =( BOUNDED_CURVE ( )  B_SPLINE_CURVE ( 2, ( #6025, #11973, #17653, #14704, #10607, #2892, #15006, #1341, #8848 ),
 .UNSPECIFIED., .F., .F. ) 
 B_SPLINE_CURVE_WITH_KNOTS ( ( 3, 2, 2, 2, 3 ),
 ( 0.4375000000000000555, 0.4444444444444444198, 0.4583333333333333148, 0.4722222222222222099, 0.4791666666666666297 ),
 .UNSPECIFIED. ) 
 CURVE ( )  GEOMETRIC_REPRESENTATION_ITEM ( )  RATIONAL_B_SPLINE_CURVE ( ( 0.9330127018922192983, 0.9330127018922198534, 1.000000000000000000, 0.8660254037844387076, 1.000000000000000000, 0.8660254037844387076, 1.000000000000000000, 0.9330127018922196314, 0.9330127018922194093 ) ) 
 REPRESENTATION_ITEM ( '' )  );
#19107 = AXIS2_PLACEMENT_3D ( 'NONE', #15842, #6765, #2351 ) ;
#19108 = CARTESIAN_POINT ( 'NONE',  ( 231.2217848218749339, -33.21562499938547575, 102.3871387122750889 ) ) ;
#19109 = CARTESIAN_POINT ( 'NONE',  ( 81.70916641599872321, -34.99999999999998579, -97.11314983874012796 ) ) ;
#19110 = CARTESIAN_POINT ( 'NONE',  ( -83.90000000000000568, -33.52106250001229171, 102.5980762113533018 ) ) ;
#19111 = CARTESIAN_POINT ( 'NONE',  ( -83.90000000000000568, -34.57500000000000284, 97.40192378864668399 ) ) ;
#19112 = CARTESIAN_POINT ( 'NONE',  ( 233.5451393107506988, -32.00000000000000711, -47.24663084804295465 ) ) ;
#19113 = CARTESIAN_POINT ( 'NONE',  ( -79.64356964375001269, -32.57812499938548001, 98.40857419181659793 ) ) ;
#19114 = CARTESIAN_POINT ( 'NONE',  ( -79.39999999999999147, -32.45624999877097139, -98.26794919243113213 ) ) ;
#19115 = CARTESIAN_POINT ( 'NONE',  ( 79.64356964375001269, -31.41562499938548569, 98.40857419181659793 ) ) ;
#19116 = LINE ( 'NONE', #14611, #3966 ) ;
#19117 = DIRECTION ( 'NONE',  ( 0.000000000000000000, -0.000000000000000000, 1.000000000000000000 ) ) ;
#19118 = CARTESIAN_POINT ( 'NONE',  ( 85.15643035624999868, -32.91562499938549280, -101.5914258081833879 ) ) ;
#19119 = CARTESIAN_POINT ( 'NONE',  ( -83.77821517812500929, -31.67812499938548498, -102.3871387122750889 ) ) ;
#19120 = AXIS2_PLACEMENT_3D ( 'NONE', #1209, #10003, #17433 ) ;
#19121 = ORIENTED_EDGE ( 'NONE', *, *, #16573, .T. ) ;
#19122 = CARTESIAN_POINT ( 'NONE',  ( 83.90000000000000568, -33.46874999877096712, 97.40192378864668399 ) ) ;
#19123 = CARTESIAN_POINT ( 'NONE',  ( 232.6775203606193543, -35.00000000000000000, -47.23891671615874088 ) ) ;
#19124 = DIRECTION ( 'NONE',  ( 0.000000000000000000, 0.000000000000000000, 1.000000000000000000 ) ) ;
#19125 = CARTESIAN_POINT ( 'NONE',  ( 235.5999999999999943, -34.18124999877096570, 98.26794919243110371 ) ) ;
#19126 = CARTESIAN_POINT ( 'NONE',  ( 79.39999999999999147, -33.80624999877097281, -101.7320508075688537 ) ) ;
#19127 = ORIENTED_EDGE ( 'NONE', *, *, #18695, .T. ) ;
#19128 = CARTESIAN_POINT ( 'NONE',  ( -81.02178482187500208, -34.94062499938548427, -97.61286128772489690 ) ) ;
#19129 = CARTESIAN_POINT ( 'NONE',  ( 0.2175679805369840625, -1.691499766289389362, -3.500000000000000000 ) ) ;
#19130 = ORIENTED_EDGE ( 'NONE', *, *, #16871, .T. ) ;
#19131 = DIRECTION ( 'NONE',  ( 1.000000000000000000, 0.000000000000000000, 0.000000000000000000 ) ) ;
#19132 = CARTESIAN_POINT ( 'NONE',  ( -84.69813954184694182, -35.39427337414329600, -101.9283554252781272 ) ) ;
#19133 = VECTOR ( 'NONE', #11328, 1000.000000000000000 ) ;
#19134 = CARTESIAN_POINT ( 'NONE',  ( -83.92761994968563499, -32.00000000000000000, -102.3311504458614394 ) ) ;
#19135 = CARTESIAN_POINT ( 'NONE',  ( -79.39999999999999147, -31.48124999877097352, -101.7320508075688821 ) ) ;
#19136 = CARTESIAN_POINT ( 'NONE',  ( 235.3564303562499447, -31.79062499938547859, 98.40857419181659793 ) ) ;
#19137 = CARTESIAN_POINT ( 'NONE',  ( -85.40000000000000568, -30.43518749875867968, 98.26794919243111792 ) ) ;
#19138 = CARTESIAN_POINT ( 'NONE',  ( -79.64356964374999848, -32.27812499938548996, 99.99999999999998579 ) ) ;
#19139 = CARTESIAN_POINT ( 'NONE',  ( -79.64356964374999848, -32.16562499938548569, -99.99999999999998579 ) ) ;
#19140 = ADVANCED_FACE ( 'NONE', ( #14907 ), #5930, .T. ) ;
#19141 = DIRECTION ( 'NONE',  ( 0.000000000000000000, 0.000000000000000000, 1.000000000000000000 ) ) ;
#19142 = FACE_OUTER_BOUND ( 'NONE', #3880, .T. ) ;
#19143 = CARTESIAN_POINT ( 'NONE',  ( 79.39999999999999147, -32.45624999877097139, -101.7320508075688537 ) ) ;
#19144 = CARTESIAN_POINT ( 'NONE',  ( 232.5999999999999375, -32.13749999999998863, 103.4641016151377499 ) ) ;
#19145 = EDGE_CURVE ( 'NONE', #8738, #13854, #17113, .T. ) ;
#19146 = ADVANCED_FACE ( 'NONE', ( #10509 ), #3081, .F. ) ;
#19147 = EDGE_LOOP ( 'NONE', ( #901, #10143, #2727, #1326 ) ) ;
#19148 = CARTESIAN_POINT ( 'NONE',  ( 85.15643035625001289, -34.64062499938548711, -99.99999999999998579 ) ) ;
#19149 = FILL_AREA_STYLE ('',( #5583 ) ) ;
#19150 = CARTESIAN_POINT ( 'NONE',  ( 235.5999999999999943, -33.35624999877096997, 101.7320508075688537 ) ) ;
#19151 = CARTESIAN_POINT ( 'NONE',  ( 235.5999999999999375, -34.21874999877096002, -50.00000000000011369 ) ) ;
#19152 = CARTESIAN_POINT ( 'NONE',  ( -79.64356964374998427, -33.55312499938548854, 101.5914258081833879 ) ) ;
#19153 = EDGE_LOOP ( 'NONE', ( #17783, #15623, #4760, #9477 ) ) ;
#19154 = VERTEX_POINT ( 'NONE', #19319 ) ;
#19155 = DIRECTION ( 'NONE',  ( 7.222237291452147586E-32, -1.214306433183764966E-16, 1.000000000000000000 ) ) ;
#19156 = CARTESIAN_POINT ( 'NONE',  ( -82.39999999999999147, -32.98124999877096286, 102.9999999999999858 ) ) ;
#19157 = CARTESIAN_POINT ( 'NONE',  ( 4.197393957002303999, -0.4069871074557456780, -3.503767560748925813 ) ) ;
#19158 = EDGE_LOOP ( 'NONE', ( #2836, #8376, #7868, #14559, #9073, #5615 ) ) ;
#19159 = CARTESIAN_POINT ( 'NONE',  ( -6.259644161404860030E-16, -4.618802153517027165, -3.433295621305388234 ) ) ;
#19160 = CARTESIAN_POINT ( 'NONE',  ( 3.973514160553463626, -2.741076955031366502, -2.383932505289870996 ) ) ;
#19161 = CARTESIAN_POINT ( 'NONE',  ( 105.1999999999999744, -34.99999999999999289, -100.0000000000000000 ) ) ;
#19162 = ADVANCED_FACE ( 'NONE', ( #13439 ), #4294, .T. ) ;
#19163 = CARTESIAN_POINT ( 'NONE',  ( -81.02178482187500208, -34.90312499938548285, 97.61286128772489690 ) ) ;
#19164 = CARTESIAN_POINT ( 'NONE',  ( -82.39999999999999147, -31.01249999999999929, 96.53589838486223584 ) ) ;
#19165 = EDGE_CURVE ( 'NONE', #1546, #7647, #8697, .T. ) ;
#19166 = CARTESIAN_POINT ( 'NONE',  ( -81.59615242270662350, -34.63259618943234130, -103.0000000000000000 ) ) ;
#19167 = CARTESIAN_POINT ( 'NONE',  ( 99.99999999999997158, -5.200000000000008171, -100.0000000000000000 ) ) ;
#19168 = EDGE_CURVE ( 'NONE', #8464, #11929, #6119, .T. ) ;
#19169 = FACE_OUTER_BOUND ( 'NONE', #1685, .T. ) ;
#19170 = CARTESIAN_POINT ( 'NONE',  ( 83.65502553130815500, -34.99999999999999289, 97.51146709331014506 ) ) ;
#19171 = CARTESIAN_POINT ( 'NONE',  ( 235.3564303562499447, -30.77812499938547575, 98.40857419181659793 ) ) ;
#19172 = ORIENTED_EDGE ( 'NONE', *, *, #12234, .T. ) ;
#19173 = CARTESIAN_POINT ( 'NONE',  ( -81.02178482187500208, -30.89062499938548711, -97.61286128772489690 ) ) ;
#19174 = CARTESIAN_POINT ( 'NONE',  ( 0.6810597143197052450, 4.461075778259290914, -3.598441714920602053 ) ) ;
#19175 = CARTESIAN_POINT ( 'NONE',  ( 109.9999999999999432, -29.80000000000002558, -150.0000000000000000 ) ) ;
#19176 = CARTESIAN_POINT ( 'NONE',  ( 229.8435696437499303, -34.30312499938548143, 99.99999999999998579 ) ) ;
#19177 = CARTESIAN_POINT ( 'NONE',  ( -85.15643035624999868, -30.17812499938548498, 98.40857419181659793 ) ) ;
#19178 = CARTESIAN_POINT ( 'NONE',  ( 82.40000000000001990, -33.26250000000000284, 103.0000000000000000 ) ) ;
#19179 = CARTESIAN_POINT ( 'NONE',  ( 233.9782151781249411, -33.89062499938548001, -52.38713871227520968 ) ) ;
#19180 = ORIENTED_EDGE ( 'NONE', *, *, #15378, .F. ) ;
#19181 = VERTEX_POINT ( 'NONE', #10226 ) ;
#19182 = FACE_BOUND ( 'NONE', #13379, .T. ) ;
#19183 = CARTESIAN_POINT ( 'NONE',  ( -85.40000000000000568, -31.35000000000000142, 99.99999999999998579 ) ) ;
#19184 = CARTESIAN_POINT ( 'NONE',  ( 110.0000000000000000, 10.19999999999997620, -137.3499999999999943 ) ) ;
#19185 = CARTESIAN_POINT ( 'NONE',  ( 79.39999999999999147, -30.26249999999999929, 98.26794919243113213 ) ) ;
#19186 = CARTESIAN_POINT ( 'NONE',  ( 83.20384757729335945, -34.14240381056767148, -96.99999999999998579 ) ) ;
#19187 = CARTESIAN_POINT ( 'NONE',  ( 232.5999999999999375, -30.92812499938547433, 103.1828516163667899 ) ) ;
#19188 = CARTESIAN_POINT ( 'NONE',  ( 232.5999999999999943, -33.62812499938547717, -46.81714838363331666 ) ) ;
#19189 = EDGE_CURVE ( 'NONE', #13951, #5496, #10991, .T. ) ;
#19190 = EDGE_CURVE ( 'NONE', #10239, #8738, #12998, .T. ) ;
#19191 = CARTESIAN_POINT ( 'NONE',  ( -80.90000000000000568, -30.60000000000000142, 97.40192378864668399 ) ) ;
#19192 = CARTESIAN_POINT ( 'NONE',  ( 81.02178482187500208, -34.49062499938548854, 97.61286128772489690 ) ) ;
#19193 = CARTESIAN_POINT ( 'NONE',  ( 85.15643035624999868, -31.00312499938548072, -101.5914258081833879 ) ) ;
#19194 = CARTESIAN_POINT ( 'NONE',  ( 234.0999999999999375, -31.04999999999999361, -52.59807621135342970 ) ) ;
#19195 = CARTESIAN_POINT ( 'NONE',  ( -81.02178482187500208, -34.94062499938548427, 102.3871387122750889 ) ) ;
#19196 = FACE_OUTER_BOUND ( 'NONE', #7949, .T. ) ;
#19197 = ORIENTED_EDGE ( 'NONE', *, *, #8958, .F. ) ;
#19198 = APPLICATION_CONTEXT ( 'automotive_design' ) ;
#19199 = CARTESIAN_POINT ( 'NONE',  ( 85.15643035624999868, -35.16562499938547859, 98.40857419181659793 ) ) ;
#19200 = DIRECTION ( 'NONE',  ( -0.000000000000000000, -0.000000000000000000, 1.000000000000000000 ) ) ;
#19201 = ADVANCED_FACE ( 'NONE', ( #6600 ), #6186, .T. ) ;
#19202 = CARTESIAN_POINT ( 'NONE',  ( 232.5999999999999375, -31.26562499938548356, -53.18285161636690361 ) ) ;
#19203 = CARTESIAN_POINT ( 'NONE',  ( -83.77821517812500929, -33.66562499938548569, 102.3871387122750889 ) ) ;
#19204 = ORIENTED_EDGE ( 'NONE', *, *, #10846, .T. ) ;
#19205 = LINE ( 'NONE', #13330, #14923 ) ;
#19206 = VECTOR ( 'NONE', #15403, 1000.000000000000000 ) ;
#19207 = CARTESIAN_POINT ( 'NONE',  ( 235.3564303562499447, -32.16562499938547859, 99.99999999999998579 ) ) ;
#19208 = CARTESIAN_POINT ( 'NONE',  ( 80.32125193361331128, -35.00000000000000000, -97.97655282300733859 ) ) ;
#19209 = CARTESIAN_POINT ( 'NONE',  ( -82.39999999999999147, -32.13356250001228887, 103.4641016151377499 ) ) ;
#19210 = CARTESIAN_POINT ( 'NONE',  ( 1.154929423581238118E-15, -3.202582148906733650, -1.452965002680433271 ) ) ;
#19211 = CARTESIAN_POINT ( 'NONE',  ( -83.77821517812500929, -32.76562499938548711, 102.3871387122750889 ) ) ;
#19212 = FACE_OUTER_BOUND ( 'NONE', #6462, .T. ) ;
#19213 = CARTESIAN_POINT ( 'NONE',  ( 85.15643035625001289, -32.50312499938548427, 99.99999999999998579 ) ) ;
#19214 = CARTESIAN_POINT ( 'NONE',  ( -83.20384757729337366, -32.79240381056766296, 97.00000000000000000 ) ) ;
#19215 = CYLINDRICAL_SURFACE ( 'NONE', #9633, 3.000000000000002665 ) ;
#19216 = CARTESIAN_POINT ( 'NONE',  ( 83.77821517812500929, -34.37812499938548427, -97.61286128772489690 ) ) ;
#19217 = CARTESIAN_POINT ( 'NONE',  ( -81.02178482187500208, -30.85312499938548569, -102.3871387122750889 ) ) ;
#19218 = ORIENTED_EDGE ( 'NONE', *, *, #2668, .T. ) ;
#19219 = CARTESIAN_POINT ( 'NONE',  ( 79.39999999999999147, -33.31874999877096855, 99.99999999999998579 ) ) ;
#19220 = CYLINDRICAL_SURFACE ( 'NONE', #17714, 3.000000000000002665 ) ;
#19221 = CARTESIAN_POINT ( 'NONE',  ( 85.40000000000000568, -32.68124999877097281, 101.7320508075688821 ) ) ;
#19222 = SHAPE_REPRESENTATION ( 'hex flange nut gradea_iso_ISO - 4161 - M5 - N', ( #10540 ), #17049 ) ;
#19223 = B_SPLINE_CURVE_WITH_KNOTS ( 'NONE', 3,
 ( #15206, #18245, #1915, #4862, #2013, #10906, #18342, #16772 ),
 .UNSPECIFIED., .F., .F.,
 ( 4, 2, 2, 4 ),
 ( 0.000000000000000000, 0.002450665683189818828, 0.003675998524784728459, 0.004901331366379638524 ),
 .UNSPECIFIED. ) ;
#19224 = CARTESIAN_POINT ( 'NONE',  ( -96.99999999999998579, -29.80000000000000426, -150.0000000000000000 ) ) ;
#19225 = CARTESIAN_POINT ( 'NONE',  ( 80.60346964444597972, -31.99999999999999289, 102.3251727584800648 ) ) ;
#19226 = ORIENTED_EDGE ( 'NONE', *, *, #7334, .T. ) ;
#19227 = CARTESIAN_POINT ( 'NONE',  ( -83.77821517812500929, -33.66562499938548569, -97.61286128772489690 ) ) ;
#19228 = CARTESIAN_POINT ( 'NONE',  ( 4.211399257449709665, -2.459727064652517114, -3.751161691472417736 ) ) ;
#19229 =( GEOMETRIC_REPRESENTATION_CONTEXT ( 3 ) GLOBAL_UNCERTAINTY_ASSIGNED_CONTEXT ( ( #17010 ) ) GLOBAL_UNIT_ASSIGNED_CONTEXT ( ( #703, #17682, #8489 ) ) REPRESENTATION_CONTEXT ( 'NONE', 'WORKASPACE' ) );
#19230 = EDGE_LOOP ( 'NONE', ( #19300, #11042, #7781, #4610 ) ) ;
#19231 = CARTESIAN_POINT ( 'NONE',  ( 0.000000000000000000, 0.000000000000000000, 3.469446951953614189E-15 ) ) ;
#19232 = CARTESIAN_POINT ( 'NONE',  ( -79.64356964375001269, -34.56562499938549138, -98.40857419181659793 ) ) ;
#19233 = CARTESIAN_POINT ( 'NONE',  ( -81.44903907891985284, -32.00000000000000711, -102.7404298451142353 ) ) ;
#19234 = CARTESIAN_POINT ( 'NONE',  ( -80.90000000000000568, -31.44374999877096855, -102.5980762113533018 ) ) ;
#19235 = CARTESIAN_POINT ( 'NONE',  ( 231.2217848218749339, -30.77812499938548285, 97.61286128772489690 ) ) ;
#19236 = CARTESIAN_POINT ( 'NONE',  ( -82.39999999999999147, -33.88124999877096855, 103.4641016151377499 ) ) ;
#19237 = CARTESIAN_POINT ( 'NONE',  ( -82.39999999999999147, -34.64062499938548711, 103.1828516163667899 ) ) ;
#19238 = CARTESIAN_POINT ( 'NONE',  ( -82.39999999999999147, -34.52812499938548285, -96.81714838363319586 ) ) ;
#19239 = DIRECTION ( 'NONE',  ( -0.000000000000000000, -1.000000000000000000, -0.000000000000000000 ) ) ;
#19240 = CARTESIAN_POINT ( 'NONE',  ( 0.000000000000000000, 4.041451884327382338, 2.749426538070117193E-16 ) ) ;
#19241 = CARTESIAN_POINT ( 'NONE',  ( 79.39999999999999147, -31.03124999877097068, -98.26794919243110371 ) ) ;
#19242 = CARTESIAN_POINT ( 'NONE',  ( 229.5999999999999375, -33.14999999999999147, 99.99999999999998579 ) ) ;
#19243 = PRODUCT_DEFINITION_FORMATION_WITH_SPECIFIED_SOURCE ( 'ANY', '', #11388, .NOT_KNOWN. ) ;
#19244 = ORIENTED_EDGE ( 'NONE', *, *, #16994, .F. ) ;
#19245 = FACE_OUTER_BOUND ( 'NONE', #19158, .T. ) ;
#19246 = SURFACE_STYLE_FILL_AREA ( #19053 ) ;
#19247 = CARTESIAN_POINT ( 'NONE',  ( 232.5999999999999375, -34.78124999877096002, 103.4641016151377499 ) ) ;
#19248 = CARTESIAN_POINT ( 'NONE',  ( 229.5999999999999375, -34.48124999877096286, -51.73205080756898866 ) ) ;
#19249 = CARTESIAN_POINT ( 'NONE',  ( -81.02178482187500208, -33.44062499938548427, 97.61286128772489690 ) ) ;
#19250 = EDGE_LOOP ( 'NONE', ( #14375, #11336, #10280, #9944, #2533 ) ) ;
#19251 = ORIENTED_EDGE ( 'NONE', *, *, #18924, .F. ) ;
#19252 = CARTESIAN_POINT ( 'NONE',  ( -83.30522522564109522, -32.00000000000000000, 97.33297554273082142 ) ) ;
#19253 = CARTESIAN_POINT ( 'NONE',  ( -81.59615242270662350, -34.31115380933863435, 102.9999999999999716 ) ) ;
#19254 = CARTESIAN_POINT ( 'NONE',  ( 232.5999999999999091, -34.38749999999999574, -47.00000000000011369 ) ) ;
#19255 = VERTEX_POINT ( 'NONE', #10794 ) ;
#19256 = CYLINDRICAL_SURFACE ( 'NONE', #16076, 2.100000000000000089 ) ;
#19257 = CARTESIAN_POINT ( 'NONE',  ( 85.40000000000000568, -34.08749999999999858, -98.26794919243111792 ) ) ;
#19258 = CARTESIAN_POINT ( 'NONE',  ( 233.4038475772933339, -32.38259618943233420, 97.00000000000000000 ) ) ;
#19259 = ADVANCED_FACE ( 'NONE', ( #12455 ), #18374, .F. ) ;
#19260 = CARTESIAN_POINT ( 'NONE',  ( -82.39999999999999147, -33.96562499938548285, 96.81714838363319586 ) ) ;
#19261 = CARTESIAN_POINT ( 'NONE',  ( -79.39999999999999147, -32.02500000000000568, 99.99999999999998579 ) ) ;
#19262 = CARTESIAN_POINT ( 'NONE',  ( -79.39999999999999147, -32.38124999877096855, 98.26794919243110371 ) ) ;
#19263 = CIRCLE ( 'NONE', #2709, 2.200000000000007283 ) ;
#19264 = DIRECTION ( 'NONE',  ( -0.000000000000000000, -1.000000000000000000, -0.000000000000000000 ) ) ;
#19265 = CARTESIAN_POINT ( 'NONE',  ( -84.69814078818293979, -35.03295773984034867, 98.07164606005757435 ) ) ;
#19266 = CARTESIAN_POINT ( 'NONE',  ( -81.59615242270662350, -34.76115380933863719, -96.99999999999995737 ) ) ;
#19267 = CARTESIAN_POINT ( 'NONE',  ( 232.5999999999999375, -30.25312499938548072, 96.81714838363319586 ) ) ;
#19268 = ORIENTED_EDGE ( 'NONE', *, *, #18961, .T. ) ;
#19269 = AXIS2_PLACEMENT_3D ( 'NONE', #17008, #12510, #3525 ) ;
#19270 = DIRECTION ( 'NONE',  ( 0.000000000000000000, 0.000000000000000000, 1.000000000000000000 ) ) ;
#19271 = CARTESIAN_POINT ( 'NONE',  ( -79.64356964374999848, -30.36562499938548498, -99.99999999999998579 ) ) ;
#19272 = CARTESIAN_POINT ( 'NONE',  ( 0.5449313310647804220, 4.304185902836899835, -3.316620875263383894 ) ) ;
#19273 = EDGE_CURVE ( 'NONE', #609, #422, #18483, .T. ) ;
#19274 = DIRECTION ( 'NONE',  ( -0.000000000000000000, -1.000000000000000000, 0.000000000000000000 ) ) ;
#19275 =( BOUNDED_CURVE ( )  B_SPLINE_CURVE ( 2, ( #5289, #15542, #8114, #5094, #12602, #18673, #3903, #3614, #12893, #13709, #3804, #11236, #12247, #796, #18214, #18574, #14162, #9773, #17394, #6853, #11039, #2341, #17199, #9869, #8303, #12798, #9207, #3712, #18765, #8399, #17003, #11333, #14067, #15639, #7754, #14351, #2443, #9575, #702, #11133, #5387, #6754, #17298, #6657, #2245, #14256, #5187, #9678, #11432, #17101, #8213, #12699, #15832, #987, #6943, #18864, #5486, #15172, #5762, #7221, #13176, #7131, #10157, #14736, #19052, #17584, #7413, #2827, #16119, #1273, #5957, #11906, #19148, #7317, #8488, #12989, #4195, #14834, #1459, #13375, #1371, #13271, #2728 ),
 .UNSPECIFIED., .F., .F. ) 
 B_SPLINE_CURVE_WITH_KNOTS ( ( 3, 2, 2, 2, 2, 2, 2, 2, 2, 2, 2, 2, 2, 2, 2, 2, 2, 2, 2, 2, 2, 2, 2, 2, 2, 2, 2, 2, 2, 2, 2, 2, 2, 2, 2, 2, 2, 2, 2, 2, 2, 3 ),
 ( 0.3716916592825992294, 0.3750191855951752751, 0.3900199530189822905, 0.4050207204427893060, 0.4200214878665963214, 0.4350222552904033368, 0.4500230227142103523, 0.4650237901380173677, 0.4800245575618243277, 0.4950253249856313431, 0.5100260924094383030, 0.5250268598332453740, 0.5400276272570523339, 0.5550283946808594049, 0.5700291621046664758, 0.5850299295284733248, 0.6000306969522805067, 0.6150314643760874667, 0.6300322317998945376, 0.6450329992237013865, 0.6600337666475084575, 0.6750345340713155284, 0.6900353014951223773, 0.7050360689189295593, 0.7200368363427365193, 0.7350376037665435902, 0.7500383711903504391, 0.7650391386141575101, 0.7800399060379645810, 0.7950406734617716520, 0.8100414408855785009, 0.8250422083093855719, 0.8400429757331926428, 0.8550437431569994917, 0.8700445105808066737, 0.8850452780046136336, 0.9000460454284207046, 0.9150468128522275535, 0.9300475802760348465, 0.9450483476998416954, 0.9600491151236487664, 0.9717223562348820121 ),
 .UNSPECIFIED. ) 
 CURVE ( )  GEOMETRIC_REPRESENTATION_ITEM ( )  RATIONAL_B_SPLINE_CURVE ( ( 0.9537471549766813883, 0.9702812541832683824, 1.000000000000000000, 0.8660254037844387076, 1.000000000000000000, 0.8660254037844387076, 1.000000000000000000, 0.8660254037844387076, 1.000000000000000000, 0.8660254037844387076, 1.000000000000000000, 0.8660254037844387076, 1.000000000000000000, 0.8660254037844387076, 1.000000000000000000, 0.8660254037844387076, 1.000000000000000000, 0.8660254037844387076, 1.000000000000000000, 0.8660254037844387076, 1.000000000000000000, 0.8660254037844387076, 1.000000000000000000, 0.8660254037844387076, 1.000000000000000000, 0.8660254037844387076, 1.000000000000000000, 0.8660254037844387076, 1.000000000000000000, 0.8660254037844387076, 1.000000000000000000, 0.8660254037844387076, 1.000000000000000000, 0.8660254037844387076, 1.000000000000000000, 0.8660254037844387076, 1.000000000000000000, 0.8660254037844387076, 1.000000000000000000, 0.8660254037844387076, 1.000000000000000000, 0.8660254037844387076, 1.000000000000000000, 0.8660254037844387076, 1.000000000000000000, 0.8660254037844387076, 1.000000000000000000, 0.8660254037844387076, 1.000000000000000000, 0.8660254037844387076, 1.000000000000000000, 0.8660254037844387076, 1.000000000000000000, 0.8660254037844387076, 1.000000000000000000, 0.8660254037844387076, 1.000000000000000000, 0.8660254037844387076, 1.000000000000000000, 0.8660254037844387076, 1.000000000000000000, 0.8660254037844387076, 1.000000000000000000, 0.8660254037844387076, 1.000000000000000000, 0.8660254037844387076, 1.000000000000000000, 0.8660254037844387076, 1.000000000000000000, 0.8660254037844387076, 1.000000000000000000, 0.8660254037844387076, 1.000000000000000000, 0.8660254037844387076, 1.000000000000000000, 0.8660254037844387076, 1.000000000000000000, 0.8660254037844387076, 1.000000000000000000, 0.8660254037844387076, 1.000000000000000000, 0.8957441496011493420, 0.9537471549767048140 ) ) 
 REPRESENTATION_ITEM ( '' )  );
#19276 = CARTESIAN_POINT ( 'NONE',  ( -83.77821517812500929, -32.01562499938548001, 97.61286128772489690 ) ) ;
#19277 = CARTESIAN_POINT ( 'NONE',  ( 79.39999999999999147, -33.41250000000000142, 98.26794919243113213 ) ) ;
#19278 = CARTESIAN_POINT ( 'NONE',  ( 235.3564303562499447, -32.20312499938548001, -48.40857419181671162 ) ) ;
#19279 = TOROIDAL_SURFACE ( 'NONE', #18956, 5.384454397937118664, 0.5155456020628804703 ) ;
#19280 = PRESENTATION_LAYER_ASSIGNMENT (  '', '', ( #7111 ) ) ;
#19281 = ORIENTED_EDGE ( 'NONE', *, *, #64, .F. ) ;
#19282 = VERTEX_POINT ( 'NONE', #5121 ) ;
#19283 = DIRECTION ( 'NONE',  ( -1.000000000000000000, 0.000000000000000000, 0.000000000000000000 ) ) ;
#19284 = CARTESIAN_POINT ( 'NONE',  ( -85.40000000000000568, -32.21249999999999858, 101.7320508075688679 ) ) ;
#19285 = EDGE_CURVE ( 'NONE', #13568, #4792, #15663, .T. ) ;
#19286 = CARTESIAN_POINT ( 'NONE',  ( -83.90000000000000568, -31.36874999877096926, 97.40192378864668399 ) ) ;
#19287 = CARTESIAN_POINT ( 'NONE',  ( 82.39999999999999147, -34.97812499938547859, 96.81714838363319586 ) ) ;
#19288 = CIRCLE ( 'NONE', #3973, 6.000000000000005329 ) ;
#19289 = FACE_OUTER_BOUND ( 'NONE', #9747, .T. ) ;
#19290 = CARTESIAN_POINT ( 'NONE',  ( 235.3564303562499447, -31.67812499938547788, 98.40857419181659793 ) ) ;
#19291 = CARTESIAN_POINT ( 'NONE',  ( 229.8435696437499587, -34.15312499938547575, -48.40857419181671162 ) ) ;
#19292 = AXIS2_PLACEMENT_3D ( 'NONE', #3957, #2677, #15884 ) ;
#19293 = CARTESIAN_POINT ( 'NONE',  ( 81.02178482187500208, -34.94062499938548427, 97.61286128772489690 ) ) ;
#19294 = AXIS2_PLACEMENT_3D ( 'NONE', #144, #15069, #1879 ) ;
#19295 = CARTESIAN_POINT ( 'NONE',  ( 81.02178482187500208, -31.19062499938548427, -97.61286128772489690 ) ) ;
#19296 = CARTESIAN_POINT ( 'NONE',  ( 235.3564303562499447, -34.82812499938548001, -51.59142580818350865 ) ) ;
#19297 = CARTESIAN_POINT ( 'NONE',  ( -82.05869624310423660, -34.96883842999723413, 102.9857998004475803 ) ) ;
#19298 = CARTESIAN_POINT ( 'NONE',  ( 85.15643035624999868, -32.35312499938549280, -101.5914258081833879 ) ) ;
#19299 = EDGE_CURVE ( 'NONE', #12317, #1971, #12369, .T. ) ;
#19300 = ORIENTED_EDGE ( 'NONE', *, *, #17160, .F. ) ;
#19301 = FACE_OUTER_BOUND ( 'NONE', #18863, .T. ) ;
#19302 = CARTESIAN_POINT ( 'NONE',  ( -82.40000000000000568, -50.00000000000000000, 99.99999999999998579 ) ) ;
#19303 = CARTESIAN_POINT ( 'NONE',  ( 235.3564303562499447, -31.34062499938548285, -51.59142580818350865 ) ) ;
#19304 = CARTESIAN_POINT ( 'NONE',  ( -83.90000000000000568, -31.27500000000000568, 102.5980762113533018 ) ) ;
#19305 = EDGE_LOOP ( 'NONE', ( #17451, #8402, #843, #4868 ) ) ;
#19306 = LINE ( 'NONE', #17832, #591 ) ;
#19307 = VECTOR ( 'NONE', #12337, 1000.000000000000000 ) ;
#19309 = CARTESIAN_POINT ( 'NONE',  ( 232.5999999999999943, -34.07812499938548001, 103.1828516163667899 ) ) ;
#19308 =( BOUNDED_CURVE ( )  B_SPLINE_CURVE ( 2, ( #3120, #16325, #15238, #4694, #8887, #312, #6262, #10740, #4404 ),
 .UNSPECIFIED., .F., .F. ) 
 B_SPLINE_CURVE_WITH_KNOTS ( ( 3, 2, 2, 2, 3 ),
 ( 0.6458333333333331483, 0.6527777777777777901, 0.6666666666666666297, 0.6805555555555555802, 0.6874999999999997780 ),
 .UNSPECIFIED. ) 
 CURVE ( )  GEOMETRIC_REPRESENTATION_ITEM ( )  RATIONAL_B_SPLINE_CURVE ( ( 0.9330127018922194093, 0.9330127018922177440, 1.000000000000000000, 0.8660254037844387076, 1.000000000000000000, 0.8660254037844387076, 1.000000000000000000, 0.9330127018922215187, 0.9330127018922194093 ) ) 
 REPRESENTATION_ITEM ( '' )  );
#19310 = CARTESIAN_POINT ( 'NONE',  ( 82.39999999999999147, -32.58750000000000568, -102.9999999999999858 ) ) ;
#19311 = CARTESIAN_POINT ( 'NONE',  ( -79.39999999999999147, -32.02106250001229881, 99.99999999999998579 ) ) ;
#19312 = CARTESIAN_POINT ( 'NONE',  ( 0.3126073911696462537, -4.041451884327388555, -1.676097590879904329E-16 ) ) ;
#19313 = EDGE_CURVE ( 'NONE', #15345, #1884, #8422, .T. ) ;
#19314 = CARTESIAN_POINT ( 'NONE',  ( 233.3129826252978205, -32.00000000000000000, -47.18802777794501679 ) ) ;
#19315 = CARTESIAN_POINT ( 'NONE',  ( -85.15643035624999868, -31.07812499938548356, 98.40857419181659793 ) ) ;
#19316 = CARTESIAN_POINT ( 'NONE',  ( 230.7429016803060051, -35.00000000000000711, 102.1174602701823488 ) ) ;
#19317 = CARTESIAN_POINT ( 'NONE',  ( 83.77821517812500929, -31.52812499938548996, 97.61286128772489690 ) ) ;
#19318 = CARTESIAN_POINT ( 'NONE',  ( -82.39999999999999147, -32.81250000000000000, 97.00000000000000000 ) ) ;
#19319 = CARTESIAN_POINT ( 'NONE',  ( -82.40000000000000568, -33.43124999877096570, 102.9999999999999858 ) ) ;
#19320 = CARTESIAN_POINT ( 'NONE',  ( -79.64356964374998427, -32.76562499938548711, 101.5914258081833879 ) ) ;
#19321 = CARTESIAN_POINT ( 'NONE',  ( -83.90000000000000568, -30.77268749875868181, 102.5980762113533018 ) ) ;
#19322 = NEXT_ASSEMBLY_USAGE_OCCURRENCE ( 'NAUO1', ' ', ' ', #15977, #14653, $ ) ;
#19323 = NEXT_ASSEMBLY_USAGE_OCCURRENCE ( 'NAUO2', ' ', ' ', #15977, #15861, $ ) ;
#19324 = NEXT_ASSEMBLY_USAGE_OCCURRENCE ( 'NAUO3', ' ', ' ', #15977, #18016, $ ) ;
#19325 = NEXT_ASSEMBLY_USAGE_OCCURRENCE ( 'NAUO4', ' ', ' ', #15977, #12507, $ ) ;
#19326 = NEXT_ASSEMBLY_USAGE_OCCURRENCE ( 'NAUO5', ' ', ' ', #15977, #11913, $ ) ;
#19327 = NEXT_ASSEMBLY_USAGE_OCCURRENCE ( 'NAUO6', ' ', ' ', #15977, #6427, $ ) ;
#19328 = NEXT_ASSEMBLY_USAGE_OCCURRENCE ( 'NAUO7', ' ', ' ', #15977, #12507, $ ) ;
#19329 = NEXT_ASSEMBLY_USAGE_OCCURRENCE ( 'NAUO8', ' ', ' ', #15977, #12507, $ ) ;
#19330 = NEXT_ASSEMBLY_USAGE_OCCURRENCE ( 'NAUO9', ' ', ' ', #15977, #12507, $ ) ;
#19331 = NEXT_ASSEMBLY_USAGE_OCCURRENCE ( 'NAUO10', ' ', ' ', #15977, #12507, $ ) ;
#19332 = NEXT_ASSEMBLY_USAGE_OCCURRENCE ( 'NAUO11', ' ', ' ', #15977, #12507, $ ) ;
#19333 = NEXT_ASSEMBLY_USAGE_OCCURRENCE ( 'NAUO12', ' ', ' ', #15977, #4398, $ ) ;
#19334 = NEXT_ASSEMBLY_USAGE_OCCURRENCE ( 'NAUO13', ' ', ' ', #15977, #4398, $ ) ;
#19335 = NEXT_ASSEMBLY_USAGE_OCCURRENCE ( 'NAUO14', ' ', ' ', #15977, #14778, $ ) ;
#19336 = NEXT_ASSEMBLY_USAGE_OCCURRENCE ( 'NAUO15', ' ', ' ', #15977, #14778, $ ) ;
#19337=COLOUR_RGB('Dark Blue',0.08,0.2,0.34);
#19338=FILL_AREA_STYLE_COLOUR('',#19337);
#19339=FILL_AREA_STYLE('',(#19338));
#19340=SURFACE_STYLE_FILL_AREA(#19339);
#19341=SURFACE_SIDE_STYLE('',(#19340));
#19342=SURFACE_STYLE_USAGE(.BOTH.,#19341);
#19343=PRESENTATION_STYLE_ASSIGNMENT((#19342));
#19344=COLOUR_RGB('Light Blue',0.38,0.62,0.78);
#19345=FILL_AREA_STYLE_COLOUR('',#19344);
#19346=FILL_AREA_STYLE('',(#19345));
#19347=SURFACE_STYLE_FILL_AREA(#19346);
#19348=SURFACE_SIDE_STYLE('',(#19347));
#19349=SURFACE_STYLE_USAGE(.BOTH.,#19348);
#19350=PRESENTATION_STYLE_ASSIGNMENT((#19349));
#19351=COLOUR_RGB('Sky Blue',0.24,0.69,0.87);
#19352=FILL_AREA_STYLE_COLOUR('',#19351);
#19353=FILL_AREA_STYLE('',(#19352));
#19354=SURFACE_STYLE_FILL_AREA(#19353);
#19355=SURFACE_SIDE_STYLE('',(#19354));
#19356=SURFACE_STYLE_USAGE(.BOTH.,#19355);
#19357=PRESENTATION_STYLE_ASSIGNMENT((#19356));
#19358=COLOUR_RGB('Grey',0.48,0.52,0.57);
#19359=FILL_AREA_STYLE_COLOUR('',#19358);
#19360=FILL_AREA_STYLE('',(#19359));
#19361=SURFACE_STYLE_FILL_AREA(#19360);
#19362=SURFACE_SIDE_STYLE('',(#19361));
#19363=SURFACE_STYLE_USAGE(.BOTH.,#19362);
#19364=PRESENTATION_STYLE_ASSIGNMENT((#19363));
#19365=COLOUR_RGB('Black',0.12,0.14,0.17);
#19366=FILL_AREA_STYLE_COLOUR('',#19365);
#19367=FILL_AREA_STYLE('',(#19366));
#19368=SURFACE_STYLE_FILL_AREA(#19367);
#19369=SURFACE_SIDE_STYLE('',(#19368));
#19370=SURFACE_STYLE_USAGE(.BOTH.,#19369);
#19371=PRESENTATION_STYLE_ASSIGNMENT((#19370));
#19372=COLOUR_RGB('Off White',0.89,0.88,0.83);
#19373=FILL_AREA_STYLE_COLOUR('',#19372);
#19374=FILL_AREA_STYLE('',(#19373));
#19375=SURFACE_STYLE_FILL_AREA(#19374);
#19376=SURFACE_SIDE_STYLE('',(#19375));
#19377=SURFACE_STYLE_USAGE(.BOTH.,#19376);
#19378=PRESENTATION_STYLE_ASSIGNMENT((#19377));
ENDSEC;
END-ISO-10303-21;
